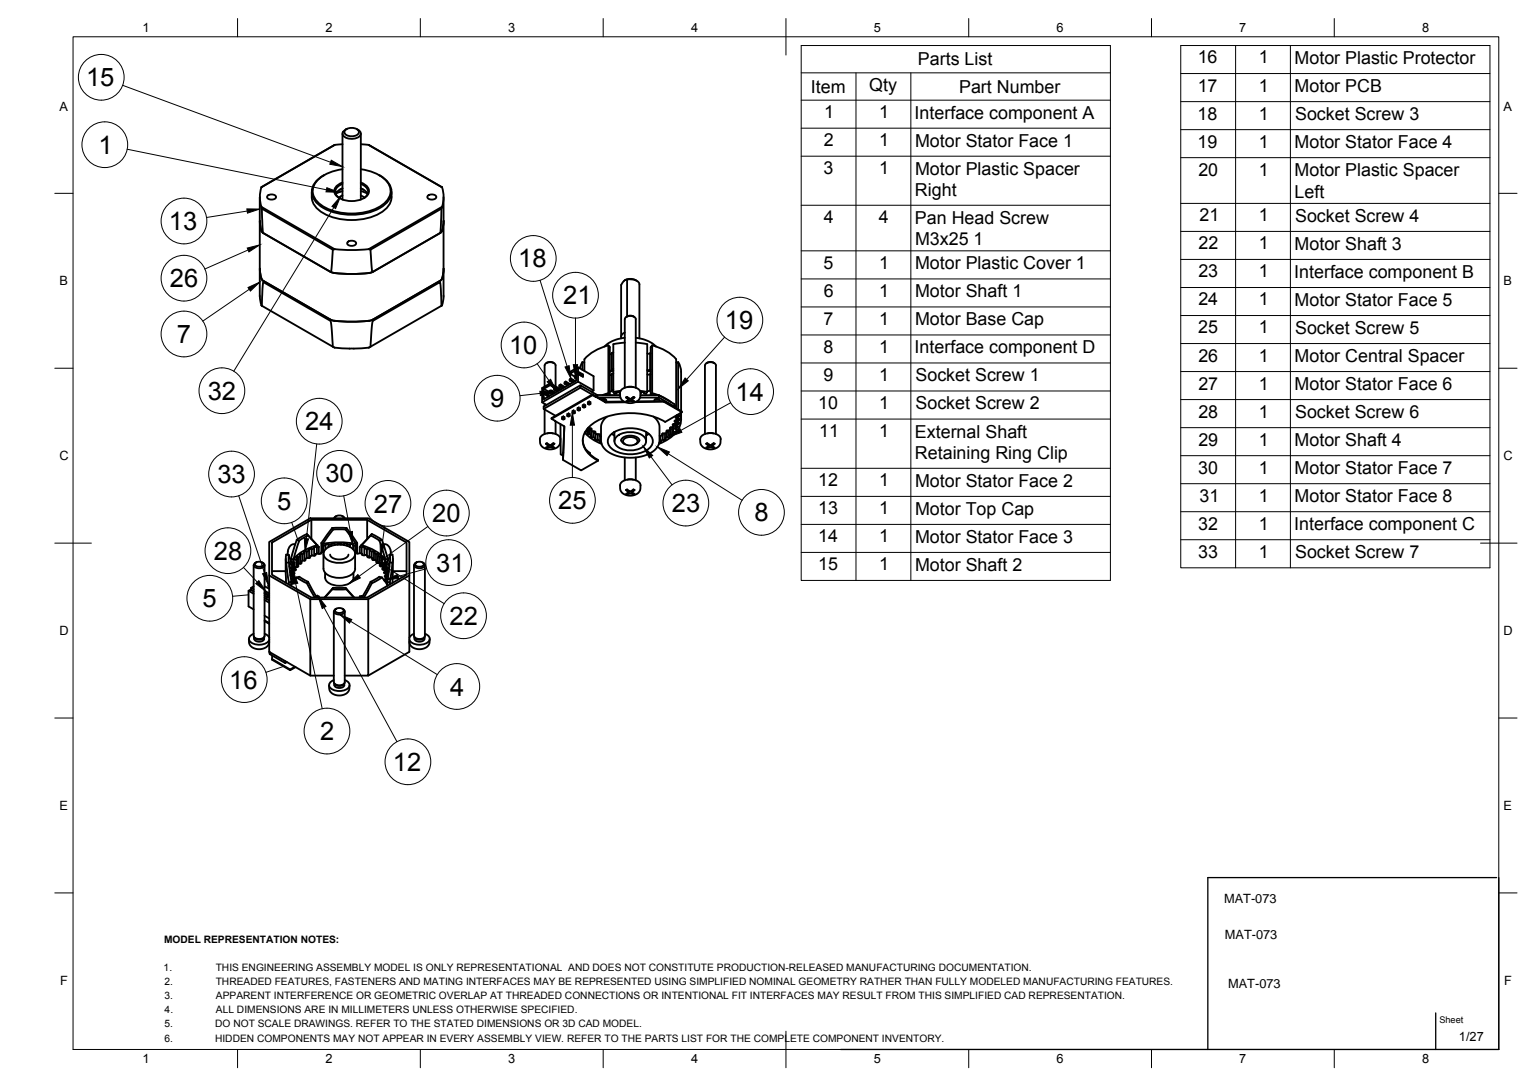
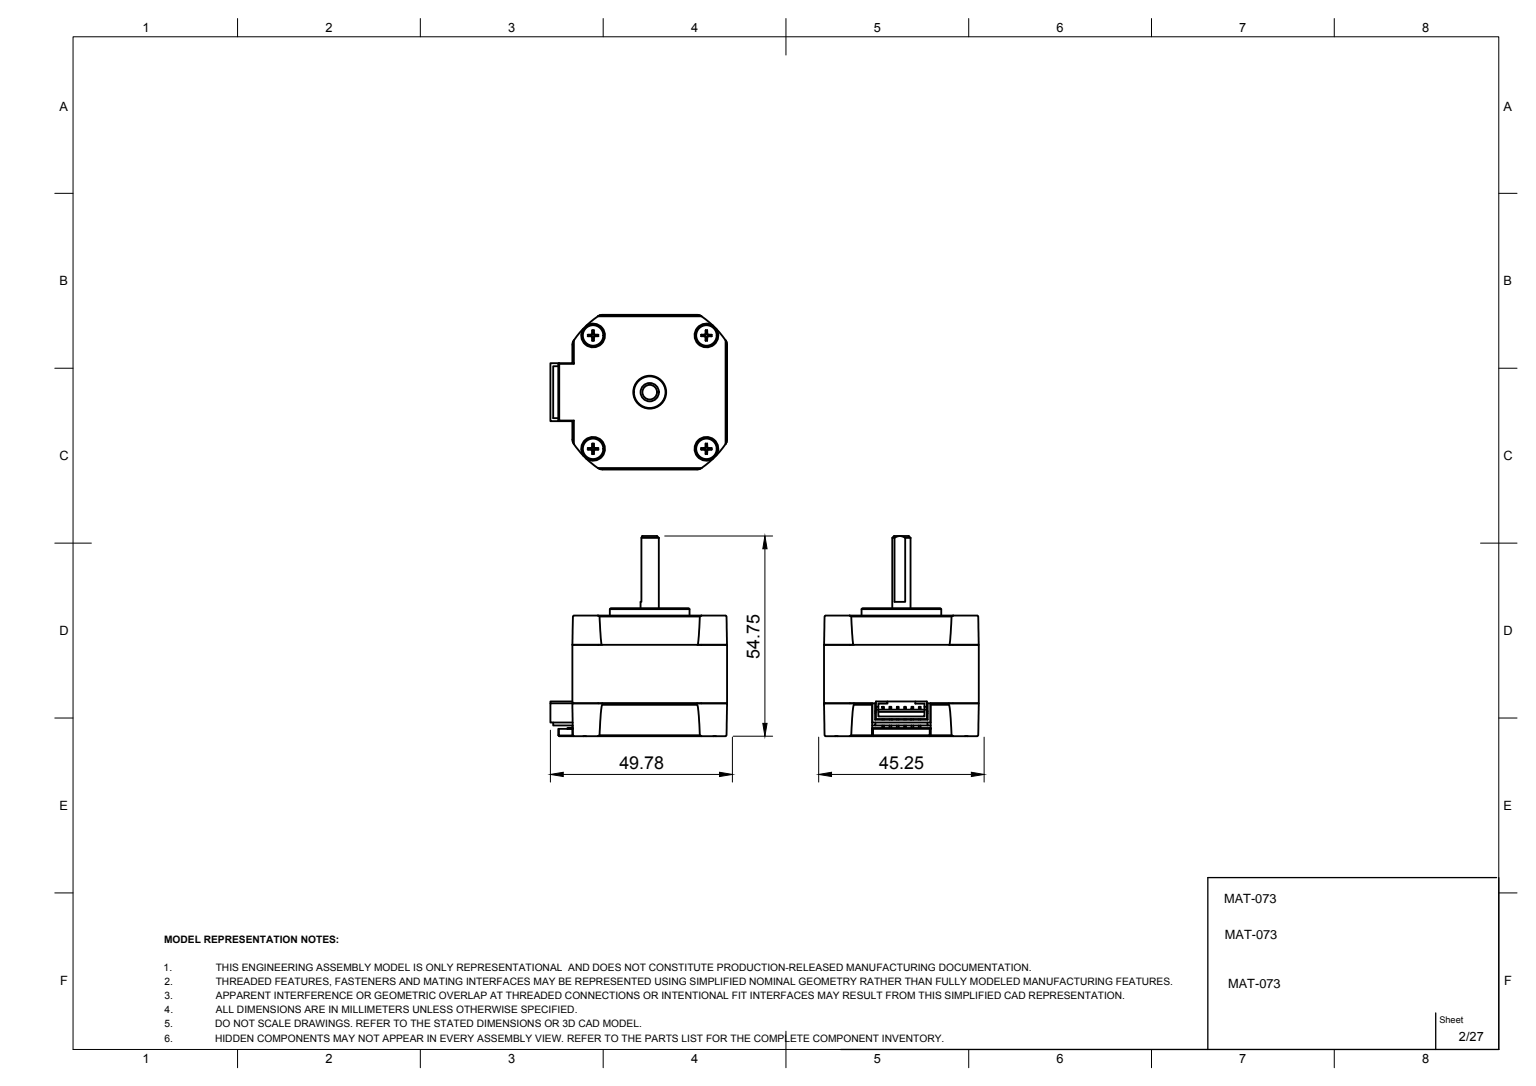
ISO-10303-21;
HEADER;
/* Generated by software containing ST-Developer
 * from STEP Tools, Inc. (www.steptools.com) 
 */

FILE_DESCRIPTION(
/* description */ ('CAx-IF Rec.Pracs.---Representation and Presentation of Product Manufa
cturing Information (PMI)---4.0---2014-10-13'),
/* implementation_level */ '2;1');

FILE_NAME(
/* name */ 'MAT-073',
/* time_stamp */ '2026-10-24T18:52:33-07:00',
/* author */ (''),
/* organization */ (''),
/* preprocessor_version */ 'ST-DEVELOPER v20.2',
/* originating_system */ 'Autodesk Translation Framework v15.17.0.0',
/* authorisation */ '');

FILE_SCHEMA (('AP242_MANAGED_MODEL_BASED_3D_ENGINEERING_MIM_LF { 1 0 10303 442 2 1 4 }'));
ENDSEC;

DATA;
#10=MECHANICAL_DESIGN_GEOMETRIC_PRESENTATION_REPRESENTATION('',(#414,#415,
#416,#417,#418,#419,#420,#421,#422,#423,#424,#425,#426,#427,#428,#429,#430,
#431,#432,#433,#434,#435,#436,#437,#438,#439,#440,#441,#442,#443,#444,#445,
#446),#34876);
#11=ITEM_DEFINED_TRANSFORMATION($,$,#19952,#22222);
#12=ITEM_DEFINED_TRANSFORMATION($,$,#19969,#22223);
#13=ITEM_DEFINED_TRANSFORMATION($,$,#20050,#22224);
#14=ITEM_DEFINED_TRANSFORMATION($,$,#22159,#22225);
#15=ITEM_DEFINED_TRANSFORMATION($,$,#20059,#22226);
#16=ITEM_DEFINED_TRANSFORMATION($,$,#20315,#22227);
#17=ITEM_DEFINED_TRANSFORMATION($,$,#20591,#22228);
#18=ITEM_DEFINED_TRANSFORMATION($,$,#20792,#22229);
#19=ITEM_DEFINED_TRANSFORMATION($,$,#20809,#22230);
#20=ITEM_DEFINED_TRANSFORMATION($,$,#20821,#22231);
#21=ITEM_DEFINED_TRANSFORMATION($,$,#20833,#22232);
#22=ITEM_DEFINED_TRANSFORMATION($,$,#20884,#22233);
#23=ITEM_DEFINED_TRANSFORMATION($,$,#20965,#22234);
#24=ITEM_DEFINED_TRANSFORMATION($,$,#21089,#22235);
#25=ITEM_DEFINED_TRANSFORMATION($,$,#21170,#22236);
#26=ITEM_DEFINED_TRANSFORMATION($,$,#21196,#22237);
#27=ITEM_DEFINED_TRANSFORMATION($,$,#21215,#22238);
#28=ITEM_DEFINED_TRANSFORMATION($,$,#21260,#22239);
#29=ITEM_DEFINED_TRANSFORMATION($,$,#21272,#22240);
#30=ITEM_DEFINED_TRANSFORMATION($,$,#21353,#22241);
#31=ITEM_DEFINED_TRANSFORMATION($,$,#21362,#22242);
#32=ITEM_DEFINED_TRANSFORMATION($,$,#21374,#22243);
#33=ITEM_DEFINED_TRANSFORMATION($,$,#21650,#22244);
#34=ITEM_DEFINED_TRANSFORMATION($,$,#21667,#22245);
#35=ITEM_DEFINED_TRANSFORMATION($,$,#21748,#22246);
#36=ITEM_DEFINED_TRANSFORMATION($,$,#21760,#22247);
#37=ITEM_DEFINED_TRANSFORMATION($,$,#21823,#22248);
#38=ITEM_DEFINED_TRANSFORMATION($,$,#21904,#22249);
#39=ITEM_DEFINED_TRANSFORMATION($,$,#21959,#22250);
#40=ITEM_DEFINED_TRANSFORMATION($,$,#21968,#22251);
#41=ITEM_DEFINED_TRANSFORMATION($,$,#22049,#22252);
#42=ITEM_DEFINED_TRANSFORMATION($,$,#22130,#22253);
#43=ITEM_DEFINED_TRANSFORMATION($,$,#22147,#22254);
#44=ITEM_DEFINED_TRANSFORMATION($,$,#22159,#22255);
#45=ITEM_DEFINED_TRANSFORMATION($,$,#22159,#22256);
#46=ITEM_DEFINED_TRANSFORMATION($,$,#22159,#22257);
#47=(
REPRESENTATION_RELATIONSHIP($,$,#34985,#34984)
REPRESENTATION_RELATIONSHIP_WITH_TRANSFORMATION(#11)
SHAPE_REPRESENTATION_RELATIONSHIP()
);
#48=(
REPRESENTATION_RELATIONSHIP($,$,#34986,#34984)
REPRESENTATION_RELATIONSHIP_WITH_TRANSFORMATION(#12)
SHAPE_REPRESENTATION_RELATIONSHIP()
);
#49=(
REPRESENTATION_RELATIONSHIP($,$,#34987,#34984)
REPRESENTATION_RELATIONSHIP_WITH_TRANSFORMATION(#13)
SHAPE_REPRESENTATION_RELATIONSHIP()
);
#50=(
REPRESENTATION_RELATIONSHIP($,$,#35017,#34984)
REPRESENTATION_RELATIONSHIP_WITH_TRANSFORMATION(#14)
SHAPE_REPRESENTATION_RELATIONSHIP()
);
#51=(
REPRESENTATION_RELATIONSHIP($,$,#34988,#34984)
REPRESENTATION_RELATIONSHIP_WITH_TRANSFORMATION(#15)
SHAPE_REPRESENTATION_RELATIONSHIP()
);
#52=(
REPRESENTATION_RELATIONSHIP($,$,#34989,#34984)
REPRESENTATION_RELATIONSHIP_WITH_TRANSFORMATION(#16)
SHAPE_REPRESENTATION_RELATIONSHIP()
);
#53=(
REPRESENTATION_RELATIONSHIP($,$,#34990,#34984)
REPRESENTATION_RELATIONSHIP_WITH_TRANSFORMATION(#17)
SHAPE_REPRESENTATION_RELATIONSHIP()
);
#54=(
REPRESENTATION_RELATIONSHIP($,$,#34991,#34984)
REPRESENTATION_RELATIONSHIP_WITH_TRANSFORMATION(#18)
SHAPE_REPRESENTATION_RELATIONSHIP()
);
#55=(
REPRESENTATION_RELATIONSHIP($,$,#34992,#34984)
REPRESENTATION_RELATIONSHIP_WITH_TRANSFORMATION(#19)
SHAPE_REPRESENTATION_RELATIONSHIP()
);
#56=(
REPRESENTATION_RELATIONSHIP($,$,#34993,#34984)
REPRESENTATION_RELATIONSHIP_WITH_TRANSFORMATION(#20)
SHAPE_REPRESENTATION_RELATIONSHIP()
);
#57=(
REPRESENTATION_RELATIONSHIP($,$,#34994,#34984)
REPRESENTATION_RELATIONSHIP_WITH_TRANSFORMATION(#21)
SHAPE_REPRESENTATION_RELATIONSHIP()
);
#58=(
REPRESENTATION_RELATIONSHIP($,$,#34995,#34984)
REPRESENTATION_RELATIONSHIP_WITH_TRANSFORMATION(#22)
SHAPE_REPRESENTATION_RELATIONSHIP()
);
#59=(
REPRESENTATION_RELATIONSHIP($,$,#34996,#34984)
REPRESENTATION_RELATIONSHIP_WITH_TRANSFORMATION(#23)
SHAPE_REPRESENTATION_RELATIONSHIP()
);
#60=(
REPRESENTATION_RELATIONSHIP($,$,#34997,#34984)
REPRESENTATION_RELATIONSHIP_WITH_TRANSFORMATION(#24)
SHAPE_REPRESENTATION_RELATIONSHIP()
);
#61=(
REPRESENTATION_RELATIONSHIP($,$,#34998,#34984)
REPRESENTATION_RELATIONSHIP_WITH_TRANSFORMATION(#25)
SHAPE_REPRESENTATION_RELATIONSHIP()
);
#62=(
REPRESENTATION_RELATIONSHIP($,$,#34999,#34984)
REPRESENTATION_RELATIONSHIP_WITH_TRANSFORMATION(#26)
SHAPE_REPRESENTATION_RELATIONSHIP()
);
#63=(
REPRESENTATION_RELATIONSHIP($,$,#35000,#34984)
REPRESENTATION_RELATIONSHIP_WITH_TRANSFORMATION(#27)
SHAPE_REPRESENTATION_RELATIONSHIP()
);
#64=(
REPRESENTATION_RELATIONSHIP($,$,#35001,#34984)
REPRESENTATION_RELATIONSHIP_WITH_TRANSFORMATION(#28)
SHAPE_REPRESENTATION_RELATIONSHIP()
);
#65=(
REPRESENTATION_RELATIONSHIP($,$,#35002,#34984)
REPRESENTATION_RELATIONSHIP_WITH_TRANSFORMATION(#29)
SHAPE_REPRESENTATION_RELATIONSHIP()
);
#66=(
REPRESENTATION_RELATIONSHIP($,$,#35003,#34984)
REPRESENTATION_RELATIONSHIP_WITH_TRANSFORMATION(#30)
SHAPE_REPRESENTATION_RELATIONSHIP()
);
#67=(
REPRESENTATION_RELATIONSHIP($,$,#35004,#34984)
REPRESENTATION_RELATIONSHIP_WITH_TRANSFORMATION(#31)
SHAPE_REPRESENTATION_RELATIONSHIP()
);
#68=(
REPRESENTATION_RELATIONSHIP($,$,#35005,#34984)
REPRESENTATION_RELATIONSHIP_WITH_TRANSFORMATION(#32)
SHAPE_REPRESENTATION_RELATIONSHIP()
);
#69=(
REPRESENTATION_RELATIONSHIP($,$,#35006,#34984)
REPRESENTATION_RELATIONSHIP_WITH_TRANSFORMATION(#33)
SHAPE_REPRESENTATION_RELATIONSHIP()
);
#70=(
REPRESENTATION_RELATIONSHIP($,$,#35007,#34984)
REPRESENTATION_RELATIONSHIP_WITH_TRANSFORMATION(#34)
SHAPE_REPRESENTATION_RELATIONSHIP()
);
#71=(
REPRESENTATION_RELATIONSHIP($,$,#35008,#34984)
REPRESENTATION_RELATIONSHIP_WITH_TRANSFORMATION(#35)
SHAPE_REPRESENTATION_RELATIONSHIP()
);
#72=(
REPRESENTATION_RELATIONSHIP($,$,#35009,#34984)
REPRESENTATION_RELATIONSHIP_WITH_TRANSFORMATION(#36)
SHAPE_REPRESENTATION_RELATIONSHIP()
);
#73=(
REPRESENTATION_RELATIONSHIP($,$,#35010,#34984)
REPRESENTATION_RELATIONSHIP_WITH_TRANSFORMATION(#37)
SHAPE_REPRESENTATION_RELATIONSHIP()
);
#74=(
REPRESENTATION_RELATIONSHIP($,$,#35011,#34984)
REPRESENTATION_RELATIONSHIP_WITH_TRANSFORMATION(#38)
SHAPE_REPRESENTATION_RELATIONSHIP()
);
#75=(
REPRESENTATION_RELATIONSHIP($,$,#35012,#34984)
REPRESENTATION_RELATIONSHIP_WITH_TRANSFORMATION(#39)
SHAPE_REPRESENTATION_RELATIONSHIP()
);
#76=(
REPRESENTATION_RELATIONSHIP($,$,#35013,#34984)
REPRESENTATION_RELATIONSHIP_WITH_TRANSFORMATION(#40)
SHAPE_REPRESENTATION_RELATIONSHIP()
);
#77=(
REPRESENTATION_RELATIONSHIP($,$,#35014,#34984)
REPRESENTATION_RELATIONSHIP_WITH_TRANSFORMATION(#41)
SHAPE_REPRESENTATION_RELATIONSHIP()
);
#78=(
REPRESENTATION_RELATIONSHIP($,$,#35015,#34984)
REPRESENTATION_RELATIONSHIP_WITH_TRANSFORMATION(#42)
SHAPE_REPRESENTATION_RELATIONSHIP()
);
#79=(
REPRESENTATION_RELATIONSHIP($,$,#35016,#34984)
REPRESENTATION_RELATIONSHIP_WITH_TRANSFORMATION(#43)
SHAPE_REPRESENTATION_RELATIONSHIP()
);
#80=(
REPRESENTATION_RELATIONSHIP($,$,#35017,#34984)
REPRESENTATION_RELATIONSHIP_WITH_TRANSFORMATION(#44)
SHAPE_REPRESENTATION_RELATIONSHIP()
);
#81=(
REPRESENTATION_RELATIONSHIP($,$,#35017,#34984)
REPRESENTATION_RELATIONSHIP_WITH_TRANSFORMATION(#45)
SHAPE_REPRESENTATION_RELATIONSHIP()
);
#82=(
REPRESENTATION_RELATIONSHIP($,$,#35017,#34984)
REPRESENTATION_RELATIONSHIP_WITH_TRANSFORMATION(#46)
SHAPE_REPRESENTATION_RELATIONSHIP()
);
#83=CONTEXT_DEPENDENT_SHAPE_REPRESENTATION(#47,#34948);
#84=CONTEXT_DEPENDENT_SHAPE_REPRESENTATION(#48,#34949);
#85=CONTEXT_DEPENDENT_SHAPE_REPRESENTATION(#49,#34950);
#86=CONTEXT_DEPENDENT_SHAPE_REPRESENTATION(#50,#34951);
#87=CONTEXT_DEPENDENT_SHAPE_REPRESENTATION(#51,#34952);
#88=CONTEXT_DEPENDENT_SHAPE_REPRESENTATION(#52,#34953);
#89=CONTEXT_DEPENDENT_SHAPE_REPRESENTATION(#53,#34954);
#90=CONTEXT_DEPENDENT_SHAPE_REPRESENTATION(#54,#34955);
#91=CONTEXT_DEPENDENT_SHAPE_REPRESENTATION(#55,#34956);
#92=CONTEXT_DEPENDENT_SHAPE_REPRESENTATION(#56,#34957);
#93=CONTEXT_DEPENDENT_SHAPE_REPRESENTATION(#57,#34958);
#94=CONTEXT_DEPENDENT_SHAPE_REPRESENTATION(#58,#34959);
#95=CONTEXT_DEPENDENT_SHAPE_REPRESENTATION(#59,#34960);
#96=CONTEXT_DEPENDENT_SHAPE_REPRESENTATION(#60,#34961);
#97=CONTEXT_DEPENDENT_SHAPE_REPRESENTATION(#61,#34962);
#98=CONTEXT_DEPENDENT_SHAPE_REPRESENTATION(#62,#34963);
#99=CONTEXT_DEPENDENT_SHAPE_REPRESENTATION(#63,#34964);
#100=CONTEXT_DEPENDENT_SHAPE_REPRESENTATION(#64,#34965);
#101=CONTEXT_DEPENDENT_SHAPE_REPRESENTATION(#65,#34966);
#102=CONTEXT_DEPENDENT_SHAPE_REPRESENTATION(#66,#34967);
#103=CONTEXT_DEPENDENT_SHAPE_REPRESENTATION(#67,#34968);
#104=CONTEXT_DEPENDENT_SHAPE_REPRESENTATION(#68,#34969);
#105=CONTEXT_DEPENDENT_SHAPE_REPRESENTATION(#69,#34970);
#106=CONTEXT_DEPENDENT_SHAPE_REPRESENTATION(#70,#34971);
#107=CONTEXT_DEPENDENT_SHAPE_REPRESENTATION(#71,#34972);
#108=CONTEXT_DEPENDENT_SHAPE_REPRESENTATION(#72,#34973);
#109=CONTEXT_DEPENDENT_SHAPE_REPRESENTATION(#73,#34974);
#110=CONTEXT_DEPENDENT_SHAPE_REPRESENTATION(#74,#34975);
#111=CONTEXT_DEPENDENT_SHAPE_REPRESENTATION(#75,#34976);
#112=CONTEXT_DEPENDENT_SHAPE_REPRESENTATION(#76,#34977);
#113=CONTEXT_DEPENDENT_SHAPE_REPRESENTATION(#77,#34978);
#114=CONTEXT_DEPENDENT_SHAPE_REPRESENTATION(#78,#34979);
#115=CONTEXT_DEPENDENT_SHAPE_REPRESENTATION(#79,#34980);
#116=CONTEXT_DEPENDENT_SHAPE_REPRESENTATION(#80,#34981);
#117=CONTEXT_DEPENDENT_SHAPE_REPRESENTATION(#81,#34982);
#118=CONTEXT_DEPENDENT_SHAPE_REPRESENTATION(#82,#34983);
#119=NEXT_ASSEMBLY_USAGE_OCCURRENCE('Interface component A:1',
'Interface component A:1','Interface component A:1',#35019,#35020,
'Interface component A:1');
#120=NEXT_ASSEMBLY_USAGE_OCCURRENCE('Motor Stator Face 1:1',
'Motor Stator Face 1:1','Motor Stator Face 1:1',#35019,#35021,
'Motor Stator Face 1:1');
#121=NEXT_ASSEMBLY_USAGE_OCCURRENCE('Motor Plastic Spacer Right:1',
'Motor Plastic Spacer Right:1','Motor Plastic Spacer Right:1',#35019,#35022,
'Motor Plastic Spacer Right:1');
#122=NEXT_ASSEMBLY_USAGE_OCCURRENCE('Pan Head Screw M3x25 1:1',
'Pan Head Screw M3x25 1:1','Pan Head Screw M3x25 1:1',#35019,#35052,
'Pan Head Screw M3x25 1:1');
#123=NEXT_ASSEMBLY_USAGE_OCCURRENCE('Motor Plastic Cover 1:1',
'Motor Plastic Cover 1:1','Motor Plastic Cover 1:1',#35019,#35023,
'Motor Plastic Cover 1:1');
#124=NEXT_ASSEMBLY_USAGE_OCCURRENCE('Motor Shaft 1:1','Motor Shaft 1:1',
'Motor Shaft 1:1',#35019,#35024,'Motor Shaft 1:1');
#125=NEXT_ASSEMBLY_USAGE_OCCURRENCE('Motor Base Cap:1',
'Motor Base Cap:1','Motor Base Cap:1',#35019,#35025,'Motor Base Cap:1');
#126=NEXT_ASSEMBLY_USAGE_OCCURRENCE('Interface component D:1',
'Interface component D:1','Interface component D:1',#35019,#35026,
'Interface component D:1');
#127=NEXT_ASSEMBLY_USAGE_OCCURRENCE('Socket Screw 1:1',
'Socket Screw 1:1','Socket Screw 1:1',#35019,#35027,'Socket Screw 1:1');
#128=NEXT_ASSEMBLY_USAGE_OCCURRENCE('Socket Screw 2:1',
'Socket Screw 2:1','Socket Screw 2:1',#35019,#35028,'Socket Screw 2:1');
#129=NEXT_ASSEMBLY_USAGE_OCCURRENCE(
'External Shaft Retaining Ring Clip:1',
'External Shaft Retaining Ring Clip:1',
'External Shaft Retaining Ring Clip:1',#35019,#35029,
'External Shaft Retaining Ring Clip:1');
#130=NEXT_ASSEMBLY_USAGE_OCCURRENCE('Motor Stator Face 2:1',
'Motor Stator Face 2:1','Motor Stator Face 2:1',#35019,#35030,
'Motor Stator Face 2:1');
#131=NEXT_ASSEMBLY_USAGE_OCCURRENCE('Motor Top Cap:1','Motor Top Cap:1',
'Motor Top Cap:1',#35019,#35031,'Motor Top Cap:1');
#132=NEXT_ASSEMBLY_USAGE_OCCURRENCE('Motor Stator Face 3:1',
'Motor Stator Face 3:1','Motor Stator Face 3:1',#35019,#35032,
'Motor Stator Face 3:1');
#133=NEXT_ASSEMBLY_USAGE_OCCURRENCE('Motor Shaft 2:1','Motor Shaft 2:1',
'Motor Shaft 2:1',#35019,#35033,'Motor Shaft 2:1');
#134=NEXT_ASSEMBLY_USAGE_OCCURRENCE('Motor Plastic Protector:1',
'Motor Plastic Protector:1','Motor Plastic Protector:1',#35019,#35034,
'Motor Plastic Protector:1');
#135=NEXT_ASSEMBLY_USAGE_OCCURRENCE('Motor PCB:1','Motor PCB:1',
'Motor PCB:1',#35019,#35035,'Motor PCB:1');
#136=NEXT_ASSEMBLY_USAGE_OCCURRENCE('Socket Screw 3:1',
'Socket Screw 3:1','Socket Screw 3:1',#35019,#35036,'Socket Screw 3:1');
#137=NEXT_ASSEMBLY_USAGE_OCCURRENCE('Motor Stator Face 4:1',
'Motor Stator Face 4:1','Motor Stator Face 4:1',#35019,#35037,
'Motor Stator Face 4:1');
#138=NEXT_ASSEMBLY_USAGE_OCCURRENCE('Motor Plastic Spacer Left:1',
'Motor Plastic Spacer Left:1','Motor Plastic Spacer Left:1',#35019,#35038,
'Motor Plastic Spacer Left:1');
#139=NEXT_ASSEMBLY_USAGE_OCCURRENCE('Socket Screw 4:1',
'Socket Screw 4:1','Socket Screw 4:1',#35019,#35039,'Socket Screw 4:1');
#140=NEXT_ASSEMBLY_USAGE_OCCURRENCE('Motor Shaft 3:1','Motor Shaft 3:1',
'Motor Shaft 3:1',#35019,#35040,'Motor Shaft 3:1');
#141=NEXT_ASSEMBLY_USAGE_OCCURRENCE('Interface component B:1',
'Interface component B:1','Interface component B:1',#35019,#35041,
'Interface component B:1');
#142=NEXT_ASSEMBLY_USAGE_OCCURRENCE('Motor Stator Face 5:1',
'Motor Stator Face 5:1','Motor Stator Face 5:1',#35019,#35042,
'Motor Stator Face 5:1');
#143=NEXT_ASSEMBLY_USAGE_OCCURRENCE('Socket Screw 5:1',
'Socket Screw 5:1','Socket Screw 5:1',#35019,#35043,'Socket Screw 5:1');
#144=NEXT_ASSEMBLY_USAGE_OCCURRENCE('Motor Central Spacer:1',
'Motor Central Spacer:1','Motor Central Spacer:1',#35019,#35044,
'Motor Central Spacer:1');
#145=NEXT_ASSEMBLY_USAGE_OCCURRENCE('Motor Stator Face 6:1',
'Motor Stator Face 6:1','Motor Stator Face 6:1',#35019,#35045,
'Motor Stator Face 6:1');
#146=NEXT_ASSEMBLY_USAGE_OCCURRENCE('Socket Screw 6:1',
'Socket Screw 6:1','Socket Screw 6:1',#35019,#35046,'Socket Screw 6:1');
#147=NEXT_ASSEMBLY_USAGE_OCCURRENCE('Motor Shaft 4:1','Motor Shaft 4:1',
'Motor Shaft 4:1',#35019,#35047,'Motor Shaft 4:1');
#148=NEXT_ASSEMBLY_USAGE_OCCURRENCE('Motor Stator Face 7:1',
'Motor Stator Face 7:1','Motor Stator Face 7:1',#35019,#35048,
'Motor Stator Face 7:1');
#149=NEXT_ASSEMBLY_USAGE_OCCURRENCE('Motor Stator Face 8:1',
'Motor Stator Face 8:1','Motor Stator Face 8:1',#35019,#35049,
'Motor Stator Face 8:1');
#150=NEXT_ASSEMBLY_USAGE_OCCURRENCE('Interface component C:1',
'Interface component C:1','Interface component C:1',#35019,#35050,
'Interface component C:1');
#151=NEXT_ASSEMBLY_USAGE_OCCURRENCE('Socket Screw 7:1',
'Socket Screw 7:1','Socket Screw 7:1',#35019,#35051,'Socket Screw 7:1');
#152=NEXT_ASSEMBLY_USAGE_OCCURRENCE('Pan Head Screw M3x25 1:2',
'Pan Head Screw M3x25 1:2','Pan Head Screw M3x25 1:2',#35019,#35052,
'Pan Head Screw M3x25 1:2');
#153=NEXT_ASSEMBLY_USAGE_OCCURRENCE('Pan Head Screw M3x25 1:3',
'Pan Head Screw M3x25 1:3','Pan Head Screw M3x25 1:3',#35019,#35052,
'Pan Head Screw M3x25 1:3');
#154=NEXT_ASSEMBLY_USAGE_OCCURRENCE('Pan Head Screw M3x25 1:4',
'Pan Head Screw M3x25 1:4','Pan Head Screw M3x25 1:4',#35019,#35052,
'Pan Head Screw M3x25 1:4');
#155=SPHERICAL_SURFACE('',#22193,0.005);
#156=(
BOUNDED_CURVE()
B_SPLINE_CURVE(2,(#31813,#31814,#31815),.UNSPECIFIED.,.F.,.F.)
B_SPLINE_CURVE_WITH_KNOTS((3,3),(0.,0.159611859165466),.UNSPECIFIED.)
CURVE()
GEOMETRIC_REPRESENTATION_ITEM()
RATIONAL_B_SPLINE_CURVE((1.,1.06066017177976,1.))
REPRESENTATION_ITEM('')
);
#157=(
BOUNDED_CURVE()
B_SPLINE_CURVE(2,(#31820,#31821,#31822),.UNSPECIFIED.,.F.,.F.)
B_SPLINE_CURVE_WITH_KNOTS((3,3),(0.159611859165466,0.319223718330933),
 .UNSPECIFIED.)
CURVE()
GEOMETRIC_REPRESENTATION_ITEM()
RATIONAL_B_SPLINE_CURVE((1.,1.06066017177976,1.))
REPRESENTATION_ITEM('')
);
#158=(
BOUNDED_CURVE()
B_SPLINE_CURVE(2,(#34461,#34462,#34463),.UNSPECIFIED.,.F.,.F.)
B_SPLINE_CURVE_WITH_KNOTS((3,3),(0.0607926731753692,0.157120419745457),
 .UNSPECIFIED.)
CURVE()
GEOMETRIC_REPRESENTATION_ITEM()
RATIONAL_B_SPLINE_CURVE((1.16988778338128,1.27990737092129,1.3120427295614))
REPRESENTATION_ITEM('')
);
#159=(
BOUNDED_CURVE()
B_SPLINE_CURVE(2,(#34466,#34467,#34468),.UNSPECIFIED.,.F.,.F.)
B_SPLINE_CURVE_WITH_KNOTS((3,3),(0.236610881719778,0.332938628428626),
 .UNSPECIFIED.)
CURVE()
GEOMETRIC_REPRESENTATION_ITEM()
RATIONAL_B_SPLINE_CURVE((1.3120427260588,1.27990736807416,1.16988778190421))
REPRESENTATION_ITEM('')
);
#160=(
BOUNDED_CURVE()
B_SPLINE_CURVE(2,(#34498,#34499,#34500),.UNSPECIFIED.,.F.,.F.)
B_SPLINE_CURVE_WITH_KNOTS((3,3),(0.060792673372948,0.15712042005291),
 .UNSPECIFIED.)
CURVE()
GEOMETRIC_REPRESENTATION_ITEM()
RATIONAL_B_SPLINE_CURVE((1.16988778221416,1.2799073686718,1.31204272679384))
REPRESENTATION_ITEM('')
);
#161=(
BOUNDED_CURVE()
B_SPLINE_CURVE(2,(#34503,#34504,#34505),.UNSPECIFIED.,.F.,.F.)
B_SPLINE_CURVE_WITH_KNOTS((3,3),(0.236610881752925,0.332938628449716),
 .UNSPECIFIED.)
CURVE()
GEOMETRIC_REPRESENTATION_ITEM()
RATIONAL_B_SPLINE_CURVE((1.3120427263507,1.27990736831095,1.16988778202699))
REPRESENTATION_ITEM('')
);
#162=(
BOUNDED_CURVE()
B_SPLINE_CURVE(2,(#34535,#34536,#34537),.UNSPECIFIED.,.F.,.F.)
B_SPLINE_CURVE_WITH_KNOTS((3,3),(0.0607926734092304,0.157120420109433),
 .UNSPECIFIED.)
CURVE()
GEOMETRIC_REPRESENTATION_ITEM()
RATIONAL_B_SPLINE_CURVE((1.1698877820014,1.27990736826137,1.31204272628854))
REPRESENTATION_ITEM('')
);
#163=(
BOUNDED_CURVE()
B_SPLINE_CURVE(2,(#34542,#34543,#34544),.UNSPECIFIED.,.F.,.F.)
B_SPLINE_CURVE_WITH_KNOTS((3,3),(0.23661088156082,0.33293862832676),
 .UNSPECIFIED.)
CURVE()
GEOMETRIC_REPRESENTATION_ITEM()
RATIONAL_B_SPLINE_CURVE((1.31204272463436,1.27990736691681,1.16988778130364))
REPRESENTATION_ITEM('')
);
#164=(
BOUNDED_CURVE()
B_SPLINE_CURVE(2,(#34574,#34575,#34576),.UNSPECIFIED.,.F.,.F.)
B_SPLINE_CURVE_WITH_KNOTS((3,3),(0.0607926733478611,0.157120420013774),
 .UNSPECIFIED.)
CURVE()
GEOMETRIC_REPRESENTATION_ITEM()
RATIONAL_B_SPLINE_CURVE((1.16988778236303,1.27990736895843,1.31204272714642))
REPRESENTATION_ITEM('')
);
#165=(
BOUNDED_CURVE()
B_SPLINE_CURVE(2,(#34579,#34580,#34581),.UNSPECIFIED.,.F.,.F.)
B_SPLINE_CURVE_WITH_KNOTS((3,3),(0.236610882341047,0.332938628827773),
 .UNSPECIFIED.)
CURVE()
GEOMETRIC_REPRESENTATION_ITEM()
RATIONAL_B_SPLINE_CURVE((1.3120427316459,1.27990737261498,1.16988778425995))
REPRESENTATION_ITEM('')
);
#166=(
BOUNDED_CURVE()
B_SPLINE_CURVE(2,(#34671,#34672,#34673),.UNSPECIFIED.,.F.,.F.)
B_SPLINE_CURVE_WITH_KNOTS((3,3),(0.167664209749899,0.177304440757115),
 .UNSPECIFIED.)
CURVE()
GEOMETRIC_REPRESENTATION_ITEM()
RATIONAL_B_SPLINE_CURVE((1.60521077046129,1.32000436275842,1.))
REPRESENTATION_ITEM('')
);
#167=(
BOUNDED_CURVE()
B_SPLINE_CURVE(2,(#34677,#34678,#34679),.UNSPECIFIED.,.F.,.F.)
B_SPLINE_CURVE_WITH_KNOTS((3,3),(0.,0.0096402310072164),.UNSPECIFIED.)
CURVE()
GEOMETRIC_REPRESENTATION_ITEM()
RATIONAL_B_SPLINE_CURVE((1.,1.32000436275842,1.60521077046128))
REPRESENTATION_ITEM('')
);
#168=(
BOUNDED_CURVE()
B_SPLINE_CURVE(2,(#34699,#34700,#34701),.UNSPECIFIED.,.F.,.F.)
B_SPLINE_CURVE_WITH_KNOTS((3,3),(0.167664209749899,0.177304440757115),
 .UNSPECIFIED.)
CURVE()
GEOMETRIC_REPRESENTATION_ITEM()
RATIONAL_B_SPLINE_CURVE((1.60521077046129,1.32000436275842,1.))
REPRESENTATION_ITEM('')
);
#169=(
BOUNDED_CURVE()
B_SPLINE_CURVE(2,(#34704,#34705,#34706),.UNSPECIFIED.,.F.,.F.)
B_SPLINE_CURVE_WITH_KNOTS((3,3),(0.167664209749899,0.177304440757115),
 .UNSPECIFIED.)
CURVE()
GEOMETRIC_REPRESENTATION_ITEM()
RATIONAL_B_SPLINE_CURVE((1.60521077046128,1.32000436275842,1.))
REPRESENTATION_ITEM('')
);
#170=(
BOUNDED_CURVE()
B_SPLINE_CURVE(2,(#34708,#34709,#34710),.UNSPECIFIED.,.F.,.F.)
B_SPLINE_CURVE_WITH_KNOTS((3,3),(0.,0.00964023100721641),.UNSPECIFIED.)
CURVE()
GEOMETRIC_REPRESENTATION_ITEM()
RATIONAL_B_SPLINE_CURVE((1.,1.32000436275842,1.60521077046128))
REPRESENTATION_ITEM('')
);
#171=(
BOUNDED_CURVE()
B_SPLINE_CURVE(2,(#34713,#34714,#34715),.UNSPECIFIED.,.F.,.F.)
B_SPLINE_CURVE_WITH_KNOTS((3,3),(0.167664209749899,0.177304440757115),
 .UNSPECIFIED.)
CURVE()
GEOMETRIC_REPRESENTATION_ITEM()
RATIONAL_B_SPLINE_CURVE((1.60521077046128,1.32000436275842,1.))
REPRESENTATION_ITEM('')
);
#172=(
BOUNDED_CURVE()
B_SPLINE_CURVE(2,(#34720,#34721,#34722),.UNSPECIFIED.,.F.,.F.)
B_SPLINE_CURVE_WITH_KNOTS((3,3),(0.,0.00964023100721641),.UNSPECIFIED.)
CURVE()
GEOMETRIC_REPRESENTATION_ITEM()
RATIONAL_B_SPLINE_CURVE((1.,1.32000436275842,1.60521077046128))
REPRESENTATION_ITEM('')
);
#173=(
BOUNDED_CURVE()
B_SPLINE_CURVE(2,(#34756,#34757,#34758),.UNSPECIFIED.,.F.,.F.)
B_SPLINE_CURVE_WITH_KNOTS((3,3),(0.,0.0096402310072164),.UNSPECIFIED.)
CURVE()
GEOMETRIC_REPRESENTATION_ITEM()
RATIONAL_B_SPLINE_CURVE((1.,1.32000436275842,1.60521077046128))
REPRESENTATION_ITEM('')
);
#174=CONICAL_SURFACE('',#20658,0.003125,0.785398163397447);
#175=CONICAL_SURFACE('',#20665,0.003125,0.785398163397447);
#176=CONICAL_SURFACE('',#20672,0.003125,0.785398163397447);
#177=CONICAL_SURFACE('',#20689,0.003125,0.785398163397447);
#178=CONICAL_SURFACE('',#20758,0.012875,0.785398163397446);
#179=CONICAL_SURFACE('',#20765,0.008125,0.244978663126864);
#180=CONICAL_SURFACE('',#21050,0.010775,0.785398163397447);
#181=CONICAL_SURFACE('',#21057,0.004625,0.785398163397445);
#182=CONICAL_SURFACE('',#21062,0.004625,0.785398163397443);
#183=CONICAL_SURFACE('',#21066,0.012875,0.785398163397446);
#184=CONICAL_SURFACE('',#21072,0.008125,0.244978663126864);
#185=CONICAL_SURFACE('',#21171,0.00225,0.78539816339745);
#186=CONICAL_SURFACE('',#21175,0.00225,0.78539816339745);
#187=CONICAL_SURFACE('',#21192,0.00225,0.78539816339745);
#188=CONICAL_SURFACE('',#22160,0.0013466375,0.785235177497158);
#189=CONICAL_SURFACE('',#22170,0.00111007998137123,0.462512251778497);
#190=CONICAL_SURFACE('',#22175,0.00111007998137123,0.462512251778497);
#191=CONICAL_SURFACE('',#22180,0.00111007998137123,0.462512251778497);
#192=CONICAL_SURFACE('',#22186,0.00111007998137123,0.462512251778497);
#193=CONICAL_SURFACE('',#22202,0.00277242641351798,0.0349065850398864);
#194=CONICAL_SURFACE('',#22204,0.000209529102193857,0.0872664625997164);
#195=CONICAL_SURFACE('',#22207,0.000209529102193857,0.0872664625997164);
#196=CONICAL_SURFACE('',#22213,0.000209529102193857,0.0872664625997164);
#197=CONICAL_SURFACE('',#22214,0.000209529102193857,0.0872664625997164);
#198=CONICAL_SURFACE('',#22216,0.000409956151237738,1.08210413623649);
#199=CONICAL_SURFACE('',#22221,0.0014323425,0.415478851838033);
#200=B_SPLINE_CURVE_WITH_KNOTS('',3,(#28743,#28744,#28745,#28746,#28747,
#28748,#28749,#28750,#28751,#28752,#28753,#28754,#28755,#28756,#28757,#28758,
#28759,#28760),.UNSPECIFIED.,.F.,.F.,(4,2,2,2,2,2,2,2,4),(-0.452364390465681,
-0.395818735844292,-0.339273081222902,-0.282727638227872,-0.226182195232841,
-0.16963675223781,-0.113091309242778,-0.0565456546213892,0.),
 .UNSPECIFIED.);
#201=B_SPLINE_CURVE_WITH_KNOTS('',3,(#28763,#28764,#28765,#28766,#28767,
#28768,#28769,#28770,#28771,#28772,#28773,#28774,#28775,#28776,#28777,#28778,
#28779,#28780),.UNSPECIFIED.,.F.,.F.,(4,2,2,2,2,2,2,2,4),(-0.904728780931361,
-0.848183126309972,-0.791637471688583,-0.735092028693552,-0.678546585698521,
-0.62200114270349,-0.565455699708459,-0.50891004508707,-0.452364390465681),
 .UNSPECIFIED.);
#202=B_SPLINE_CURVE_WITH_KNOTS('',3,(#28851,#28852,#28853,#28854,#28855,
#28856,#28857,#28858,#28859,#28860,#28861,#28862,#28863,#28864,#28865,#28866,
#28867,#28868),.UNSPECIFIED.,.F.,.F.,(4,2,2,2,2,2,2,2,4),(-0.452364390465681,
-0.395818735844292,-0.339273081222903,-0.282727638227872,-0.22618219523284,
-0.169636752237809,-0.113091309242778,-0.0565456546213892,0.),
 .UNSPECIFIED.);
#203=B_SPLINE_CURVE_WITH_KNOTS('',3,(#28871,#28872,#28873,#28874,#28875,
#28876,#28877,#28878,#28879,#28880,#28881,#28882,#28883,#28884,#28885,#28886,
#28887,#28888),.UNSPECIFIED.,.F.,.F.,(4,2,2,2,2,2,2,2,4),(-0.904728780931361,
-0.848183126309972,-0.791637471688583,-0.735092028693552,-0.678546585698521,
-0.622001142703489,-0.565455699708458,-0.508910045087069,-0.45236439046568),
 .UNSPECIFIED.);
#204=B_SPLINE_CURVE_WITH_KNOTS('',3,(#28959,#28960,#28961,#28962,#28963,
#28964,#28965,#28966,#28967,#28968,#28969,#28970,#28971,#28972,#28973,#28974,
#28975,#28976),.UNSPECIFIED.,.F.,.F.,(4,2,2,2,2,2,2,2,4),(-0.452364390465681,
-0.395818735844292,-0.339273081222902,-0.282727638227871,-0.22618219523284,
-0.169636752237809,-0.113091309242778,-0.0565456546213892,0.),
 .UNSPECIFIED.);
#205=B_SPLINE_CURVE_WITH_KNOTS('',3,(#28979,#28980,#28981,#28982,#28983,
#28984,#28985,#28986,#28987,#28988,#28989,#28990,#28991,#28992,#28993,#28994,
#28995,#28996),.UNSPECIFIED.,.F.,.F.,(4,2,2,2,2,2,2,2,4),(-0.904728780931362,
-0.848183126309972,-0.791637471688583,-0.735092028693552,-0.678546585698521,
-0.62200114270349,-0.565455699708459,-0.50891004508707,-0.452364390465681),
 .UNSPECIFIED.);
#206=B_SPLINE_CURVE_WITH_KNOTS('',3,(#29067,#29068,#29069,#29070,#29071,
#29072,#29073,#29074,#29075,#29076,#29077,#29078,#29079,#29080,#29081,#29082,
#29083,#29084),.UNSPECIFIED.,.F.,.F.,(4,2,2,2,2,2,2,2,4),(-0.452364390465681,
-0.395818735844292,-0.339273081222903,-0.282727638227872,-0.226182195232841,
-0.169636752237809,-0.113091309242778,-0.0565456546213892,0.),
 .UNSPECIFIED.);
#207=B_SPLINE_CURVE_WITH_KNOTS('',3,(#29087,#29088,#29089,#29090,#29091,
#29092,#29093,#29094,#29095,#29096,#29097,#29098,#29099,#29100,#29101,#29102,
#29103,#29104),.UNSPECIFIED.,.F.,.F.,(4,2,2,2,2,2,2,2,4),(-0.904728780931362,
-0.848183126309973,-0.791637471688583,-0.735092028693552,-0.678546585698521,
-0.62200114270349,-0.565455699708459,-0.50891004508707,-0.452364390465681),
 .UNSPECIFIED.);
#208=B_SPLINE_CURVE_WITH_KNOTS('',3,(#29175,#29176,#29177,#29178,#29179,
#29180,#29181,#29182,#29183,#29184,#29185,#29186,#29187,#29188,#29189,#29190,
#29191,#29192),.UNSPECIFIED.,.F.,.F.,(4,2,2,2,2,2,2,2,4),(-0.452364390465681,
-0.395818735844292,-0.339273081222903,-0.282727638227872,-0.226182195232841,
-0.169636752237809,-0.113091309242778,-0.0565456546213892,0.),
 .UNSPECIFIED.);
#209=B_SPLINE_CURVE_WITH_KNOTS('',3,(#29195,#29196,#29197,#29198,#29199,
#29200,#29201,#29202,#29203,#29204,#29205,#29206,#29207,#29208,#29209,#29210,
#29211,#29212),.UNSPECIFIED.,.F.,.F.,(4,2,2,2,2,2,2,2,4),(-0.904728780931362,
-0.848183126309973,-0.791637471688584,-0.735092028693553,-0.678546585698522,
-0.62200114270349,-0.565455699708459,-0.50891004508707,-0.452364390465681),
 .UNSPECIFIED.);
#210=B_SPLINE_CURVE_WITH_KNOTS('',3,(#29283,#29284,#29285,#29286,#29287,
#29288,#29289,#29290,#29291,#29292,#29293,#29294,#29295,#29296,#29297,#29298,
#29299,#29300),.UNSPECIFIED.,.F.,.F.,(4,2,2,2,2,2,2,2,4),(-0.452364390465681,
-0.395818735844292,-0.339273081222903,-0.282727638227872,-0.22618219523284,
-0.169636752237809,-0.113091309242778,-0.0565456546213891,0.),
 .UNSPECIFIED.);
#211=B_SPLINE_CURVE_WITH_KNOTS('',3,(#29303,#29304,#29305,#29306,#29307,
#29308,#29309,#29310,#29311,#29312,#29313,#29314,#29315,#29316,#29317,#29318,
#29319,#29320),.UNSPECIFIED.,.F.,.F.,(4,2,2,2,2,2,2,2,4),(-0.904728780931362,
-0.848183126309973,-0.791637471688583,-0.735092028693552,-0.678546585698521,
-0.62200114270349,-0.565455699708459,-0.50891004508707,-0.452364390465681),
 .UNSPECIFIED.);
#212=B_SPLINE_CURVE_WITH_KNOTS('',3,(#29391,#29392,#29393,#29394,#29395,
#29396,#29397,#29398,#29399,#29400,#29401,#29402,#29403,#29404,#29405,#29406,
#29407,#29408),.UNSPECIFIED.,.F.,.F.,(4,2,2,2,2,2,2,2,4),(-0.452364390465681,
-0.395818735844292,-0.339273081222902,-0.282727638227872,-0.226182195232841,
-0.169636752237809,-0.113091309242778,-0.0565456546213892,0.),
 .UNSPECIFIED.);
#213=B_SPLINE_CURVE_WITH_KNOTS('',3,(#29411,#29412,#29413,#29414,#29415,
#29416,#29417,#29418,#29419,#29420,#29421,#29422,#29423,#29424,#29425,#29426,
#29427,#29428),.UNSPECIFIED.,.F.,.F.,(4,2,2,2,2,2,2,2,4),(-0.904728780931362,
-0.848183126309973,-0.791637471688583,-0.735092028693552,-0.678546585698521,
-0.62200114270349,-0.565455699708459,-0.50891004508707,-0.452364390465681),
 .UNSPECIFIED.);
#214=B_SPLINE_CURVE_WITH_KNOTS('',3,(#29499,#29500,#29501,#29502,#29503,
#29504,#29505,#29506,#29507,#29508,#29509,#29510,#29511,#29512,#29513,#29514,
#29515,#29516),.UNSPECIFIED.,.F.,.F.,(4,2,2,2,2,2,2,2,4),(-0.452364390465681,
-0.395818735844292,-0.339273081222903,-0.282727638227872,-0.226182195232841,
-0.169636752237809,-0.113091309242778,-0.0565456546213892,0.),
 .UNSPECIFIED.);
#215=B_SPLINE_CURVE_WITH_KNOTS('',3,(#29519,#29520,#29521,#29522,#29523,
#29524,#29525,#29526,#29527,#29528,#29529,#29530,#29531,#29532,#29533,#29534,
#29535,#29536),.UNSPECIFIED.,.F.,.F.,(4,2,2,2,2,2,2,2,4),(-0.904728780931362,
-0.848183126309973,-0.791637471688583,-0.735092028693552,-0.678546585698521,
-0.62200114270349,-0.565455699708459,-0.50891004508707,-0.452364390465681),
 .UNSPECIFIED.);
#216=B_SPLINE_CURVE_WITH_KNOTS('',3,(#30332,#30333,#30334,#30335,#30336,
#30337),.UNSPECIFIED.,.F.,.F.,(4,2,4),(1.58777834959488,1.67090244580867,
1.70100758687363),.UNSPECIFIED.);
#217=B_SPLINE_CURVE_WITH_KNOTS('',3,(#30373,#30374,#30375,#30376,#30377,
#30378),.UNSPECIFIED.,.F.,.F.,(4,2,4),(1.58777834958732,1.67090244580931,
1.70100758688213),.UNSPECIFIED.);
#218=B_SPLINE_CURVE_WITH_KNOTS('',3,(#30414,#30415,#30416,#30417,#30418,
#30419),.UNSPECIFIED.,.F.,.F.,(4,2,4),(1.58777834957897,1.67090244581023,
1.70100758689154),.UNSPECIFIED.);
#219=B_SPLINE_CURVE_WITH_KNOTS('',3,(#30471,#30472,#30473,#30474,#30475,
#30476),.UNSPECIFIED.,.F.,.F.,(4,2,4),(1.58777834959617,1.67090244580851,
1.70100758687202),.UNSPECIFIED.);
#220=B_SPLINE_CURVE_WITH_KNOTS('',3,(#34435,#34436,#34437,#34438,#34439,
#34440,#34441,#34442,#34443,#34444),.UNSPECIFIED.,.F.,.F.,(4,2,2,2,4),(0.0294844094794275,
0.0320672178808003,0.0352683618118342,0.0385150894591433,0.0409598490463399),
 .UNSPECIFIED.);
#221=B_SPLINE_CURVE_WITH_KNOTS('',3,(#34448,#34449,#34450,#34451,#34452,
#34453,#34454,#34455,#34456,#34457),.UNSPECIFIED.,.F.,.F.,(4,2,2,2,4),(0.0104731770181891,
0.0129179366053853,0.0161646642526944,0.0193658081837281,0.0219486165852225),
 .UNSPECIFIED.);
#222=B_SPLINE_CURVE_WITH_KNOTS('',3,(#34472,#34473,#34474,#34475,#34476,
#34477,#34478,#34479,#34480,#34481),.UNSPECIFIED.,.F.,.F.,(4,2,2,2,4),(0.0294844112755818,
0.0320672196769547,0.0352683636079885,0.0385150912552978,0.0409598508424944),
 .UNSPECIFIED.);
#223=B_SPLINE_CURVE_WITH_KNOTS('',3,(#34485,#34486,#34487,#34488,#34489,
#34490,#34491,#34492,#34493,#34494),.UNSPECIFIED.,.F.,.F.,(4,2,2,2,4),(0.0104731770181892,
0.0129179366053856,0.0161646642526945,0.0193658081837283,0.0219486165852223),
 .UNSPECIFIED.);
#224=B_SPLINE_CURVE_WITH_KNOTS('',3,(#34509,#34510,#34511,#34512,#34513,
#34514,#34515,#34516,#34517,#34518),.UNSPECIFIED.,.F.,.F.,(4,2,2,2,4),(0.0294844112754596,
0.0320672196769543,0.0352683636079882,0.0385150912552974,0.040959850842494),
 .UNSPECIFIED.);
#225=B_SPLINE_CURVE_WITH_KNOTS('',3,(#34522,#34523,#34524,#34525,#34526,
#34527,#34528,#34529,#34530,#34531),.UNSPECIFIED.,.F.,.F.,(4,2,2,2,4),(0.0104731770181891,
0.0129179366053853,0.0161646642526943,0.0193658081837282,0.0219486165851014),
 .UNSPECIFIED.);
#226=B_SPLINE_CURVE_WITH_KNOTS('',3,(#34548,#34549,#34550,#34551,#34552,
#34553,#34554,#34555,#34556,#34557),.UNSPECIFIED.,.F.,.F.,(4,2,2,2,4),(0.029484409479306,
0.0320672178808001,0.0352683618118339,0.038515089459143,0.0409598490463398),
 .UNSPECIFIED.);
#227=B_SPLINE_CURVE_WITH_KNOTS('',3,(#34561,#34562,#34563,#34564,#34565,
#34566,#34567,#34568,#34569,#34570),.UNSPECIFIED.,.F.,.F.,(4,2,2,2,4),(0.0104731770181892,
0.0129179366053856,0.0161646642526945,0.0193658081837283,0.0219486165851011),
 .UNSPECIFIED.);
#228=B_SPLINE_CURVE_WITH_KNOTS('',3,(#34594,#34595,#34596,#34597,#34598,
#34599,#34600,#34601,#34602,#34603),.UNSPECIFIED.,.F.,.F.,(4,2,2,2,4),(0.0992219002317977,
0.105487377923686,0.113471050376119,0.121445475099517,0.129419899822916),
 .UNSPECIFIED.);
#229=B_SPLINE_CURVE_WITH_KNOTS('',3,(#34608,#34609,#34610,#34611,#34612,
#34613,#34614,#34615,#34616,#34617),.UNSPECIFIED.,.F.,.F.,(4,2,2,2,4),(0.0992219004931051,
0.105487378184993,0.113471050637426,0.121445475360824,0.129419900084223),
 .UNSPECIFIED.);
#230=B_SPLINE_CURVE_WITH_KNOTS('',3,(#34622,#34623,#34624,#34625,#34626,
#34627,#34628,#34629,#34630,#34631),.UNSPECIFIED.,.F.,.F.,(4,2,2,2,4),(0.099221900231798,
0.105487377923686,0.113471050376119,0.121445475099517,0.129419899822916),
 .UNSPECIFIED.);
#231=B_SPLINE_CURVE_WITH_KNOTS('',3,(#34636,#34637,#34638,#34639,#34640,
#34641,#34642,#34643,#34644,#34645),.UNSPECIFIED.,.F.,.F.,(4,2,2,2,4),(0.0992219004931048,
0.105487378184993,0.113471050637426,0.121445475360825,0.129419900084223),
 .UNSPECIFIED.);
#232=B_SPLINE_CURVE_WITH_KNOTS('',3,(#34655,#34656,#34657,#34658,#34659,
#34660,#34661,#34662,#34663,#34664,#34665,#34666,#34667,#34668),
 .UNSPECIFIED.,.F.,.F.,(4,2,2,2,2,2,4),(0.00869408947528055,0.0191036740231402,
0.0270432080340005,0.0349827420448608,0.0429222760557212,0.0508618100665816,
0.0612713946144406),.UNSPECIFIED.);
#233=B_SPLINE_CURVE_WITH_KNOTS('',3,(#34683,#34684,#34685,#34686,#34687,
#34688,#34689,#34690,#34691,#34692,#34693,#34694,#34695,#34696),
 .UNSPECIFIED.,.F.,.F.,(4,2,2,2,2,2,4),(0.00869408947528055,0.0191036740231402,
0.0270432080340005,0.0349827420448608,0.0429222760557211,0.0508618100665814,
0.061271394614441),.UNSPECIFIED.);
#234=B_SPLINE_CURVE_WITH_KNOTS('',3,(#34724,#34725,#34726,#34727,#34728,
#34729,#34730,#34731,#34732,#34733,#34734,#34735,#34736,#34737),
 .UNSPECIFIED.,.F.,.F.,(4,2,2,2,2,2,4),(0.00869408947528073,0.0191036740231402,
0.0270432080340005,0.0349827420448608,0.0429222760557212,0.0508618100665817,
0.0612713946144409),.UNSPECIFIED.);
#235=B_SPLINE_CURVE_WITH_KNOTS('',3,(#34740,#34741,#34742,#34743,#34744,
#34745,#34746,#34747,#34748,#34749,#34750,#34751,#34752,#34753),
 .UNSPECIFIED.,.F.,.F.,(4,2,2,2,2,2,4),(0.00869408947528071,0.0191036740231402,
0.0270432080340005,0.0349827420448608,0.0429222760557211,0.0508618100665814,
0.0612713946144409),.UNSPECIFIED.);
#236=ELLIPSE('',#20061,0.0264106630927894,0.0146500000000133);
#237=ELLIPSE('',#20063,0.0264106630927895,0.0146500000000133);
#238=ELLIPSE('',#20064,0.0264106630927895,0.0146500000000133);
#239=ELLIPSE('',#20066,0.0264106630927894,0.0146500000000133);
#240=ELLIPSE('',#20069,0.0250585813644904,0.0139000000000133);
#241=ELLIPSE('',#20073,0.0250585813644904,0.0139000000000133);
#242=ELLIPSE('',#20076,0.0250585813644904,0.0139000000000133);
#243=ELLIPSE('',#20078,0.0250585813644904,0.0139000000000133);
#244=ELLIPSE('',#20089,0.0264106630927891,0.0146500000000128);
#245=ELLIPSE('',#20091,0.0264106630927891,0.0146500000000128);
#246=ELLIPSE('',#20092,0.0264106630927891,0.0146500000000128);
#247=ELLIPSE('',#20094,0.0264106630927891,0.0146500000000128);
#248=ELLIPSE('',#20097,0.0250585813644901,0.0139000000000128);
#249=ELLIPSE('',#20101,0.0250585813644901,0.0139000000000128);
#250=ELLIPSE('',#20104,0.0250585813644901,0.0139000000000128);
#251=ELLIPSE('',#20106,0.0250585813644901,0.0139000000000128);
#252=ELLIPSE('',#20117,0.0264106630927895,0.0146500000000133);
#253=ELLIPSE('',#20119,0.0264106630927894,0.0146500000000133);
#254=ELLIPSE('',#20120,0.0264106630927894,0.0146500000000133);
#255=ELLIPSE('',#20122,0.0264106630927895,0.0146500000000133);
#256=ELLIPSE('',#20125,0.0250585813644904,0.0139000000000133);
#257=ELLIPSE('',#20129,0.0250585813644904,0.0139000000000133);
#258=ELLIPSE('',#20132,0.0250585813644904,0.0139000000000133);
#259=ELLIPSE('',#20134,0.0250585813644904,0.0139000000000133);
#260=ELLIPSE('',#20145,0.0264106630927891,0.0146500000000128);
#261=ELLIPSE('',#20147,0.0264106630927891,0.0146500000000128);
#262=ELLIPSE('',#20148,0.0264106630927891,0.0146500000000128);
#263=ELLIPSE('',#20150,0.0264106630927891,0.0146500000000128);
#264=ELLIPSE('',#20153,0.0250585813644901,0.0139000000000128);
#265=ELLIPSE('',#20157,0.0250585813644901,0.0139000000000128);
#266=ELLIPSE('',#20160,0.0250585813644901,0.0139000000000128);
#267=ELLIPSE('',#20162,0.0250585813644901,0.0139000000000128);
#268=ELLIPSE('',#20173,0.0264106630927894,0.0146500000000133);
#269=ELLIPSE('',#20175,0.0264106630927895,0.0146500000000133);
#270=ELLIPSE('',#20176,0.0264106630927894,0.0146500000000133);
#271=ELLIPSE('',#20178,0.0264106630927894,0.0146500000000133);
#272=ELLIPSE('',#20181,0.0250585813644904,0.0139000000000133);
#273=ELLIPSE('',#20185,0.0250585813644904,0.0139000000000133);
#274=ELLIPSE('',#20188,0.0250585813644904,0.0139000000000133);
#275=ELLIPSE('',#20190,0.0250585813644904,0.0139000000000133);
#276=ELLIPSE('',#20201,0.0264106630927891,0.0146500000000128);
#277=ELLIPSE('',#20203,0.0264106630927891,0.0146500000000128);
#278=ELLIPSE('',#20204,0.0264106630927891,0.0146500000000128);
#279=ELLIPSE('',#20206,0.0264106630927891,0.0146500000000128);
#280=ELLIPSE('',#20209,0.0250585813644901,0.0139000000000128);
#281=ELLIPSE('',#20213,0.0250585813644901,0.0139000000000128);
#282=ELLIPSE('',#20216,0.0250585813644901,0.0139000000000128);
#283=ELLIPSE('',#20218,0.0250585813644901,0.0139000000000128);
#284=ELLIPSE('',#20229,0.0264106630927895,0.0146500000000133);
#285=ELLIPSE('',#20231,0.0264106630927894,0.0146500000000133);
#286=ELLIPSE('',#20232,0.0264106630927894,0.0146500000000133);
#287=ELLIPSE('',#20234,0.0264106630927895,0.0146500000000133);
#288=ELLIPSE('',#20237,0.0250585813644904,0.0139000000000133);
#289=ELLIPSE('',#20241,0.0250585813644904,0.0139000000000133);
#290=ELLIPSE('',#20244,0.0250585813644904,0.0139000000000133);
#291=ELLIPSE('',#20246,0.0250585813644904,0.0139000000000133);
#292=ELLIPSE('',#20257,0.0264106630927891,0.0146500000000128);
#293=ELLIPSE('',#20259,0.0264106630927891,0.0146500000000128);
#294=ELLIPSE('',#20260,0.0264106630927891,0.0146500000000128);
#295=ELLIPSE('',#20262,0.0264106630927891,0.0146500000000128);
#296=ELLIPSE('',#20265,0.0250585813644901,0.0139000000000128);
#297=ELLIPSE('',#20269,0.0250585813644901,0.0139000000000128);
#298=ELLIPSE('',#20272,0.0250585813644901,0.0139000000000128);
#299=ELLIPSE('',#20274,0.0250585813644901,0.0139000000000128);
#300=ELLIPSE('',#20594,0.114597376996511,0.00199999999998973);
#301=ELLIPSE('',#20596,0.00280406412973375,0.00199999999998973);
#302=ELLIPSE('',#20598,0.0352260556299788,0.0251250000000126);
#303=ELLIPSE('',#20600,0.0352260556299788,0.0251250000000126);
#304=ELLIPSE('',#20604,0.00280406412976774,0.00200000000001397);
#305=ELLIPSE('',#20606,0.114597376997899,0.00200000000001397);
#306=ELLIPSE('',#20609,0.114597376996524,0.00199999999998997);
#307=ELLIPSE('',#20611,0.00280406412973409,0.00199999999998997);
#308=ELLIPSE('',#20613,0.0352260556299805,0.0251250000000138);
#309=ELLIPSE('',#20615,0.0352260556299805,0.0251250000000138);
#310=ELLIPSE('',#20619,0.00280406412974482,0.00199999999999762);
#311=ELLIPSE('',#20621,0.114597376996964,0.00199999999999762);
#312=ELLIPSE('',#20624,0.114597376997842,0.00200000000001296);
#313=ELLIPSE('',#20626,0.00280406412976633,0.00200000000001296);
#314=ELLIPSE('',#20628,0.0352260556299806,0.0251250000000138);
#315=ELLIPSE('',#20630,0.0352260556299803,0.0251250000000138);
#316=ELLIPSE('',#20638,0.00280406412973409,0.00199999999998998);
#317=ELLIPSE('',#20639,0.114597376996526,0.00199999999998998);
#318=ELLIPSE('',#20642,0.0352260556300019,0.0251250000000291);
#319=ELLIPSE('',#20645,0.0352260556300016,0.0251250000000291);
#320=ELLIPSE('',#20648,0.114597376997269,0.00200000000000295);
#321=ELLIPSE('',#20649,0.00280406412975229,0.00200000000000295);
#322=ELLIPSE('',#20653,0.114597376996301,0.00199999999998605);
#323=ELLIPSE('',#20654,0.00280406412972858,0.00199999999998605);
#324=ELLIPSE('',#20968,0.00280406412975229,0.00200000000000295);
#325=ELLIPSE('',#20969,0.114597376997271,0.00200000000000295);
#326=ELLIPSE('',#20972,0.0352260556300016,0.0251250000000291);
#327=ELLIPSE('',#20974,0.0352260556300019,0.0251250000000291);
#328=ELLIPSE('',#20977,0.00280406412976774,0.00200000000001397);
#329=ELLIPSE('',#20978,0.114597376997902,0.00200000000001397);
#330=ELLIPSE('',#20981,0.0352260556299788,0.0251250000000126);
#331=ELLIPSE('',#20983,0.0352260556299788,0.0251250000000126);
#332=ELLIPSE('',#20986,0.00280406412974482,0.00199999999999762);
#333=ELLIPSE('',#20987,0.114597376996966,0.00199999999999762);
#334=ELLIPSE('',#20990,0.0352260556299805,0.0251250000000138);
#335=ELLIPSE('',#20992,0.0352260556299805,0.0251250000000138);
#336=ELLIPSE('',#20995,0.00280406412972858,0.00199999999998605);
#337=ELLIPSE('',#20996,0.114597376996303,0.00199999999998605);
#338=ELLIPSE('',#20999,0.0352260556299806,0.0251250000000138);
#339=ELLIPSE('',#21001,0.0352260556299803,0.0251250000000138);
#340=ELLIPSE('',#21004,0.114597376996528,0.00199999999998998);
#341=ELLIPSE('',#21005,0.00280406412973409,0.00199999999998998);
#342=ELLIPSE('',#21008,0.114597376996513,0.00199999999998973);
#343=ELLIPSE('',#21009,0.00280406412973375,0.00199999999998973);
#344=ELLIPSE('',#21012,0.114597376996527,0.00199999999998997);
#345=ELLIPSE('',#21013,0.00280406412973409,0.00199999999998997);
#346=ELLIPSE('',#21016,0.114597376997844,0.00200000000001296);
#347=ELLIPSE('',#21017,0.00280406412976633,0.00200000000001296);
#348=SHAPE_REPRESENTATION_RELATIONSHIP('SRR','None',#34985,#381);
#349=SHAPE_REPRESENTATION_RELATIONSHIP('SRR','None',#34986,#382);
#350=SHAPE_REPRESENTATION_RELATIONSHIP('SRR','None',#34987,#383);
#351=SHAPE_REPRESENTATION_RELATIONSHIP('SRR','None',#34988,#384);
#352=SHAPE_REPRESENTATION_RELATIONSHIP('SRR','None',#34989,#385);
#353=SHAPE_REPRESENTATION_RELATIONSHIP('SRR','None',#34990,#386);
#354=SHAPE_REPRESENTATION_RELATIONSHIP('SRR','None',#34991,#387);
#355=SHAPE_REPRESENTATION_RELATIONSHIP('SRR','None',#34992,#388);
#356=SHAPE_REPRESENTATION_RELATIONSHIP('SRR','None',#34993,#389);
#357=SHAPE_REPRESENTATION_RELATIONSHIP('SRR','None',#34994,#390);
#358=SHAPE_REPRESENTATION_RELATIONSHIP('SRR','None',#34995,#391);
#359=SHAPE_REPRESENTATION_RELATIONSHIP('SRR','None',#34996,#392);
#360=SHAPE_REPRESENTATION_RELATIONSHIP('SRR','None',#34997,#393);
#361=SHAPE_REPRESENTATION_RELATIONSHIP('SRR','None',#34998,#394);
#362=SHAPE_REPRESENTATION_RELATIONSHIP('SRR','None',#34999,#395);
#363=SHAPE_REPRESENTATION_RELATIONSHIP('SRR','None',#35000,#396);
#364=SHAPE_REPRESENTATION_RELATIONSHIP('SRR','None',#35001,#397);
#365=SHAPE_REPRESENTATION_RELATIONSHIP('SRR','None',#35002,#398);
#366=SHAPE_REPRESENTATION_RELATIONSHIP('SRR','None',#35003,#399);
#367=SHAPE_REPRESENTATION_RELATIONSHIP('SRR','None',#35004,#400);
#368=SHAPE_REPRESENTATION_RELATIONSHIP('SRR','None',#35005,#401);
#369=SHAPE_REPRESENTATION_RELATIONSHIP('SRR','None',#35006,#402);
#370=SHAPE_REPRESENTATION_RELATIONSHIP('SRR','None',#35007,#403);
#371=SHAPE_REPRESENTATION_RELATIONSHIP('SRR','None',#35008,#404);
#372=SHAPE_REPRESENTATION_RELATIONSHIP('SRR','None',#35009,#405);
#373=SHAPE_REPRESENTATION_RELATIONSHIP('SRR','None',#35010,#406);
#374=SHAPE_REPRESENTATION_RELATIONSHIP('SRR','None',#35011,#407);
#375=SHAPE_REPRESENTATION_RELATIONSHIP('SRR','None',#35012,#408);
#376=SHAPE_REPRESENTATION_RELATIONSHIP('SRR','None',#35013,#409);
#377=SHAPE_REPRESENTATION_RELATIONSHIP('SRR','None',#35014,#410);
#378=SHAPE_REPRESENTATION_RELATIONSHIP('SRR','None',#35015,#411);
#379=SHAPE_REPRESENTATION_RELATIONSHIP('SRR','None',#35016,#412);
#380=SHAPE_REPRESENTATION_RELATIONSHIP('SRR','None',#35017,#413);
#381=ADVANCED_BREP_SHAPE_REPRESENTATION('',(#447),#34843);
#382=ADVANCED_BREP_SHAPE_REPRESENTATION('',(#448),#34844);
#383=ADVANCED_BREP_SHAPE_REPRESENTATION('',(#449),#34845);
#384=ADVANCED_BREP_SHAPE_REPRESENTATION('',(#450),#34846);
#385=ADVANCED_BREP_SHAPE_REPRESENTATION('',(#451),#34847);
#386=ADVANCED_BREP_SHAPE_REPRESENTATION('',(#452),#34848);
#387=ADVANCED_BREP_SHAPE_REPRESENTATION('',(#453),#34849);
#388=ADVANCED_BREP_SHAPE_REPRESENTATION('',(#454),#34850);
#389=ADVANCED_BREP_SHAPE_REPRESENTATION('',(#455),#34851);
#390=ADVANCED_BREP_SHAPE_REPRESENTATION('',(#456),#34852);
#391=ADVANCED_BREP_SHAPE_REPRESENTATION('',(#457),#34853);
#392=ADVANCED_BREP_SHAPE_REPRESENTATION('',(#458),#34854);
#393=ADVANCED_BREP_SHAPE_REPRESENTATION('',(#459),#34855);
#394=ADVANCED_BREP_SHAPE_REPRESENTATION('',(#460),#34856);
#395=ADVANCED_BREP_SHAPE_REPRESENTATION('',(#461),#34857);
#396=ADVANCED_BREP_SHAPE_REPRESENTATION('',(#462),#34858);
#397=ADVANCED_BREP_SHAPE_REPRESENTATION('',(#463),#34859);
#398=ADVANCED_BREP_SHAPE_REPRESENTATION('',(#464),#34860);
#399=ADVANCED_BREP_SHAPE_REPRESENTATION('',(#465),#34861);
#400=ADVANCED_BREP_SHAPE_REPRESENTATION('',(#466),#34862);
#401=ADVANCED_BREP_SHAPE_REPRESENTATION('',(#467),#34863);
#402=ADVANCED_BREP_SHAPE_REPRESENTATION('',(#468),#34864);
#403=ADVANCED_BREP_SHAPE_REPRESENTATION('',(#469),#34865);
#404=ADVANCED_BREP_SHAPE_REPRESENTATION('',(#470),#34866);
#405=ADVANCED_BREP_SHAPE_REPRESENTATION('',(#471),#34867);
#406=ADVANCED_BREP_SHAPE_REPRESENTATION('',(#472),#34868);
#407=ADVANCED_BREP_SHAPE_REPRESENTATION('',(#473),#34869);
#408=ADVANCED_BREP_SHAPE_REPRESENTATION('',(#474),#34870);
#409=ADVANCED_BREP_SHAPE_REPRESENTATION('',(#475),#34871);
#410=ADVANCED_BREP_SHAPE_REPRESENTATION('',(#476),#34872);
#411=ADVANCED_BREP_SHAPE_REPRESENTATION('',(#477),#34873);
#412=ADVANCED_BREP_SHAPE_REPRESENTATION('',(#478),#34874);
#413=ADVANCED_BREP_SHAPE_REPRESENTATION('',(#479),#34875);
#414=STYLED_ITEM('',(#35159),#447);
#415=STYLED_ITEM('',(#35160),#448);
#416=STYLED_ITEM('',(#35161),#449);
#417=STYLED_ITEM('',(#35162),#450);
#418=STYLED_ITEM('',(#35163),#451);
#419=STYLED_ITEM('',(#35159),#452);
#420=STYLED_ITEM('',(#35161),#453);
#421=STYLED_ITEM('',(#35164),#454);
#422=STYLED_ITEM('',(#35165),#455);
#423=STYLED_ITEM('',(#35159),#456);
#424=STYLED_ITEM('',(#35166),#457);
#425=STYLED_ITEM('',(#35162),#458);
#426=STYLED_ITEM('',(#35163),#459);
#427=STYLED_ITEM('',(#35159),#460);
#428=STYLED_ITEM('',(#35160),#461);
#429=STYLED_ITEM('',(#35161),#462);
#430=STYLED_ITEM('',(#35164),#463);
#431=STYLED_ITEM('',(#35162),#464);
#432=STYLED_ITEM('',(#35159),#465);
#433=STYLED_ITEM('',(#35166),#466);
#434=STYLED_ITEM('',(#35161),#467);
#435=STYLED_ITEM('',(#35163),#468);
#436=STYLED_ITEM('',(#35165),#469);
#437=STYLED_ITEM('',(#35159),#470);
#438=STYLED_ITEM('',(#35166),#471);
#439=STYLED_ITEM('',(#35160),#472);
#440=STYLED_ITEM('',(#35161),#473);
#441=STYLED_ITEM('',(#35164),#474);
#442=STYLED_ITEM('',(#35162),#475);
#443=STYLED_ITEM('',(#35163),#476);
#444=STYLED_ITEM('',(#35165),#477);
#445=STYLED_ITEM('',(#35159),#478);
#446=STYLED_ITEM('',(#35164),#479);
#447=MANIFOLD_SOLID_BREP('Dowel Pin 5x16 Long 1',#19554);
#448=MANIFOLD_SOLID_BREP('Motor Stator Face 1',#19555);
#449=MANIFOLD_SOLID_BREP('Motor Plastic Spacer Right',#19556);
#450=MANIFOLD_SOLID_BREP('Motor Plastic Cover 1',#19557);
#451=MANIFOLD_SOLID_BREP('Motor Shaft 1',#19558);
#452=MANIFOLD_SOLID_BREP('Motor Base Cap',#19559);
#453=MANIFOLD_SOLID_BREP('Dowel Pin 5x16 1',#19560);
#454=MANIFOLD_SOLID_BREP('Socket Screw 1',#19561);
#455=MANIFOLD_SOLID_BREP('Socket Screw 2',#19562);
#456=MANIFOLD_SOLID_BREP('External Shaft Retaining Ring Clip',#19563);
#457=MANIFOLD_SOLID_BREP('Motor Stator Face 2',#19564);
#458=MANIFOLD_SOLID_BREP('Motor Top Cap',#19565);
#459=MANIFOLD_SOLID_BREP('Motor Stator Face 3',#19566);
#460=MANIFOLD_SOLID_BREP('Motor Shaft 2',#19567);
#461=MANIFOLD_SOLID_BREP('Motor Plastic Protector',#19568);
#462=MANIFOLD_SOLID_BREP('Motor PCB',#19569);
#463=MANIFOLD_SOLID_BREP('Socket Screw 3',#19570);
#464=MANIFOLD_SOLID_BREP('Motor Stator Face 4',#19571);
#465=MANIFOLD_SOLID_BREP('Motor Plastic Spacer Left',#19572);
#466=MANIFOLD_SOLID_BREP('Socket Screw 4',#19573);
#467=MANIFOLD_SOLID_BREP('Motor Shaft 3',#19574);
#468=MANIFOLD_SOLID_BREP('Dowel Pin 5x16 2',#19575);
#469=MANIFOLD_SOLID_BREP('Motor Stator Face 5',#19576);
#470=MANIFOLD_SOLID_BREP('Socket Screw 5',#19577);
#471=MANIFOLD_SOLID_BREP('Motor Central Spacer',#19578);
#472=MANIFOLD_SOLID_BREP('Motor Stator Face 6',#19579);
#473=MANIFOLD_SOLID_BREP('Socket Screw 6',#19580);
#474=MANIFOLD_SOLID_BREP('Motor Shaft 4',#19581);
#475=MANIFOLD_SOLID_BREP('Motor Stator Face 7',#19582);
#476=MANIFOLD_SOLID_BREP('Motor Stator Face 8',#19583);
#477=MANIFOLD_SOLID_BREP('Dowel Pin 5x16 Long 2',#19584);
#478=MANIFOLD_SOLID_BREP('Socket Screw 7',#19585);
#479=MANIFOLD_SOLID_BREP('Pan Head Screw M3x25 1',#19586);
#480=FACE_BOUND('',#5841,.T.);
#481=FACE_BOUND('',#5844,.T.);
#482=FACE_BOUND('',#5883,.T.);
#483=FACE_BOUND('',#5887,.T.);
#484=FACE_BOUND('',#5889,.T.);
#485=FACE_BOUND('',#5904,.T.);
#486=FACE_BOUND('',#5919,.T.);
#487=FACE_BOUND('',#5934,.T.);
#488=FACE_BOUND('',#5949,.T.);
#489=FACE_BOUND('',#5964,.T.);
#490=FACE_BOUND('',#5979,.T.);
#491=FACE_BOUND('',#5994,.T.);
#492=FACE_BOUND('',#6009,.T.);
#493=FACE_BOUND('',#6018,.T.);
#494=FACE_BOUND('',#6020,.T.);
#495=FACE_BOUND('',#6022,.T.);
#496=FACE_BOUND('',#6024,.T.);
#497=FACE_BOUND('',#6026,.T.);
#498=FACE_BOUND('',#6028,.T.);
#499=FACE_BOUND('',#6030,.T.);
#500=FACE_BOUND('',#6032,.T.);
#501=FACE_BOUND('',#6091,.T.);
#502=FACE_BOUND('',#6138,.T.);
#503=FACE_BOUND('',#6175,.T.);
#504=FACE_BOUND('',#6184,.T.);
#505=FACE_BOUND('',#6185,.T.);
#506=FACE_BOUND('',#6186,.T.);
#507=FACE_BOUND('',#6187,.T.);
#508=FACE_BOUND('',#6224,.T.);
#509=FACE_BOUND('',#6229,.T.);
#510=FACE_BOUND('',#6232,.T.);
#511=FACE_BOUND('',#6235,.T.);
#512=FACE_BOUND('',#6238,.T.);
#513=FACE_BOUND('',#6241,.T.);
#514=FACE_BOUND('',#6242,.T.);
#515=FACE_BOUND('',#6245,.T.);
#516=FACE_BOUND('',#6247,.T.);
#517=FACE_BOUND('',#6255,.T.);
#518=FACE_BOUND('',#6258,.T.);
#519=FACE_BOUND('',#6354,.T.);
#520=FACE_BOUND('',#6355,.T.);
#521=FACE_BOUND('',#6356,.T.);
#522=FACE_BOUND('',#6357,.T.);
#523=FACE_BOUND('',#6358,.T.);
#524=FACE_BOUND('',#6361,.T.);
#525=FACE_BOUND('',#6362,.T.);
#526=FACE_BOUND('',#6363,.T.);
#527=FACE_BOUND('',#6364,.T.);
#528=FACE_BOUND('',#6365,.T.);
#529=FACE_BOUND('',#6379,.T.);
#530=FACE_BOUND('',#6383,.T.);
#531=FACE_BOUND('',#6389,.T.);
#532=FACE_BOUND('',#6392,.T.);
#533=FACE_BOUND('',#6402,.T.);
#534=FACE_BOUND('',#6448,.T.);
#535=FACE_BOUND('',#6450,.T.);
#536=FACE_BOUND('',#6495,.T.);
#537=FACE_BOUND('',#6496,.T.);
#538=FACE_BOUND('',#6497,.T.);
#539=FACE_BOUND('',#6498,.T.);
#540=FACE_BOUND('',#6499,.T.);
#541=FACE_BOUND('',#6500,.T.);
#542=FACE_BOUND('',#6501,.T.);
#543=FACE_BOUND('',#6502,.T.);
#544=FACE_BOUND('',#6503,.T.);
#545=FACE_BOUND('',#6504,.T.);
#546=FACE_BOUND('',#6506,.T.);
#547=FACE_BOUND('',#6507,.T.);
#548=FACE_BOUND('',#6508,.T.);
#549=FACE_BOUND('',#6509,.T.);
#550=FACE_BOUND('',#6510,.T.);
#551=FACE_BOUND('',#6511,.T.);
#552=FACE_BOUND('',#6512,.T.);
#553=FACE_BOUND('',#6513,.T.);
#554=FACE_BOUND('',#6514,.T.);
#555=FACE_BOUND('',#6515,.T.);
#556=FACE_BOUND('',#6562,.T.);
#557=FACE_BOUND('',#6566,.T.);
#558=FACE_BOUND('',#6621,.T.);
#559=FACE_BOUND('',#6668,.T.);
#560=FACE_BOUND('',#6674,.T.);
#561=FACE_BOUND('',#6677,.T.);
#562=FACE_BOUND('',#6740,.T.);
#563=FACE_BOUND('',#6741,.T.);
#564=FACE_BOUND('',#6742,.T.);
#565=FACE_BOUND('',#6743,.T.);
#566=FACE_BOUND('',#6744,.T.);
#567=FACE_BOUND('',#6759,.T.);
#568=FACE_BOUND('',#6760,.T.);
#569=FACE_BOUND('',#6761,.T.);
#570=FACE_BOUND('',#6762,.T.);
#571=FACE_BOUND('',#6763,.T.);
#572=FACE_BOUND('',#6831,.T.);
#573=FACE_BOUND('',#6832,.T.);
#574=FACE_BOUND('',#6833,.T.);
#575=FACE_BOUND('',#6834,.T.);
#576=FACE_BOUND('',#6835,.T.);
#577=FACE_BOUND('',#6836,.T.);
#578=FACE_BOUND('',#6858,.T.);
#579=FACE_BOUND('',#6859,.T.);
#580=FACE_BOUND('',#6860,.T.);
#581=FACE_BOUND('',#6861,.T.);
#582=FACE_BOUND('',#6862,.T.);
#583=FACE_BOUND('',#6863,.T.);
#584=FACE_BOUND('',#6869,.T.);
#585=FACE_BOUND('',#6871,.T.);
#586=FACE_BOUND('',#6947,.T.);
#587=FACE_BOUND('',#6950,.T.);
#588=FACE_BOUND('',#6974,.T.);
#589=FACE_BOUND('',#6991,.T.);
#590=PLANE('',#19961);
#591=PLANE('',#19966);
#592=PLANE('',#19979);
#593=PLANE('',#19989);
#594=PLANE('',#19999);
#595=PLANE('',#20009);
#596=PLANE('',#20019);
#597=PLANE('',#20020);
#598=PLANE('',#20021);
#599=PLANE('',#20022);
#600=PLANE('',#20023);
#601=PLANE('',#20030);
#602=PLANE('',#20040);
#603=PLANE('',#20045);
#604=PLANE('',#20048);
#605=PLANE('',#20049);
#606=PLANE('',#20051);
#607=PLANE('',#20058);
#608=PLANE('',#20067);
#609=PLANE('',#20068);
#610=PLANE('',#20070);
#611=PLANE('',#20072);
#612=PLANE('',#20074);
#613=PLANE('',#20075);
#614=PLANE('',#20080);
#615=PLANE('',#20081);
#616=PLANE('',#20082);
#617=PLANE('',#20087);
#618=PLANE('',#20095);
#619=PLANE('',#20096);
#620=PLANE('',#20098);
#621=PLANE('',#20100);
#622=PLANE('',#20102);
#623=PLANE('',#20103);
#624=PLANE('',#20108);
#625=PLANE('',#20109);
#626=PLANE('',#20110);
#627=PLANE('',#20115);
#628=PLANE('',#20123);
#629=PLANE('',#20124);
#630=PLANE('',#20126);
#631=PLANE('',#20128);
#632=PLANE('',#20130);
#633=PLANE('',#20131);
#634=PLANE('',#20136);
#635=PLANE('',#20137);
#636=PLANE('',#20138);
#637=PLANE('',#20143);
#638=PLANE('',#20151);
#639=PLANE('',#20152);
#640=PLANE('',#20154);
#641=PLANE('',#20156);
#642=PLANE('',#20158);
#643=PLANE('',#20159);
#644=PLANE('',#20164);
#645=PLANE('',#20165);
#646=PLANE('',#20166);
#647=PLANE('',#20171);
#648=PLANE('',#20179);
#649=PLANE('',#20180);
#650=PLANE('',#20182);
#651=PLANE('',#20184);
#652=PLANE('',#20186);
#653=PLANE('',#20187);
#654=PLANE('',#20192);
#655=PLANE('',#20193);
#656=PLANE('',#20194);
#657=PLANE('',#20199);
#658=PLANE('',#20207);
#659=PLANE('',#20208);
#660=PLANE('',#20210);
#661=PLANE('',#20212);
#662=PLANE('',#20214);
#663=PLANE('',#20215);
#664=PLANE('',#20220);
#665=PLANE('',#20221);
#666=PLANE('',#20222);
#667=PLANE('',#20227);
#668=PLANE('',#20235);
#669=PLANE('',#20236);
#670=PLANE('',#20238);
#671=PLANE('',#20240);
#672=PLANE('',#20242);
#673=PLANE('',#20243);
#674=PLANE('',#20248);
#675=PLANE('',#20249);
#676=PLANE('',#20250);
#677=PLANE('',#20255);
#678=PLANE('',#20263);
#679=PLANE('',#20264);
#680=PLANE('',#20266);
#681=PLANE('',#20268);
#682=PLANE('',#20270);
#683=PLANE('',#20271);
#684=PLANE('',#20276);
#685=PLANE('',#20277);
#686=PLANE('',#20278);
#687=PLANE('',#20285);
#688=PLANE('',#20286);
#689=PLANE('',#20287);
#690=PLANE('',#20288);
#691=PLANE('',#20289);
#692=PLANE('',#20290);
#693=PLANE('',#20291);
#694=PLANE('',#20292);
#695=PLANE('',#20293);
#696=PLANE('',#20294);
#697=PLANE('',#20295);
#698=PLANE('',#20296);
#699=PLANE('',#20297);
#700=PLANE('',#20298);
#701=PLANE('',#20299);
#702=PLANE('',#20300);
#703=PLANE('',#20301);
#704=PLANE('',#20302);
#705=PLANE('',#20303);
#706=PLANE('',#20304);
#707=PLANE('',#20305);
#708=PLANE('',#20306);
#709=PLANE('',#20307);
#710=PLANE('',#20308);
#711=PLANE('',#20309);
#712=PLANE('',#20310);
#713=PLANE('',#20311);
#714=PLANE('',#20312);
#715=PLANE('',#20313);
#716=PLANE('',#20314);
#717=PLANE('',#20448);
#718=PLANE('',#20586);
#719=PLANE('',#20592);
#720=PLANE('',#20607);
#721=PLANE('',#20622);
#722=PLANE('',#20633);
#723=PLANE('',#20634);
#724=PLANE('',#20635);
#725=PLANE('',#20636);
#726=PLANE('',#20655);
#727=PLANE('',#20656);
#728=PLANE('',#20657);
#729=PLANE('',#20663);
#730=PLANE('',#20664);
#731=PLANE('',#20670);
#732=PLANE('',#20671);
#733=PLANE('',#20677);
#734=PLANE('',#20678);
#735=PLANE('',#20679);
#736=PLANE('',#20680);
#737=PLANE('',#20681);
#738=PLANE('',#20699);
#739=PLANE('',#20700);
#740=PLANE('',#20708);
#741=PLANE('',#20709);
#742=PLANE('',#20710);
#743=PLANE('',#20711);
#744=PLANE('',#20712);
#745=PLANE('',#20713);
#746=PLANE('',#20714);
#747=PLANE('',#20718);
#748=PLANE('',#20722);
#749=PLANE('',#20726);
#750=PLANE('',#20730);
#751=PLANE('',#20731);
#752=PLANE('',#20732);
#753=PLANE('',#20733);
#754=PLANE('',#20736);
#755=PLANE('',#20737);
#756=PLANE('',#20741);
#757=PLANE('',#20745);
#758=PLANE('',#20749);
#759=PLANE('',#20750);
#760=PLANE('',#20751);
#761=PLANE('',#20755);
#762=PLANE('',#20756);
#763=PLANE('',#20757);
#764=PLANE('',#20761);
#765=PLANE('',#20770);
#766=PLANE('',#20773);
#767=PLANE('',#20776);
#768=PLANE('',#20779);
#769=PLANE('',#20782);
#770=PLANE('',#20786);
#771=PLANE('',#20787);
#772=PLANE('',#20788);
#773=PLANE('',#20789);
#774=PLANE('',#20790);
#775=PLANE('',#20791);
#776=PLANE('',#20801);
#777=PLANE('',#20806);
#778=PLANE('',#20810);
#779=PLANE('',#20811);
#780=PLANE('',#20815);
#781=PLANE('',#20816);
#782=PLANE('',#20817);
#783=PLANE('',#20818);
#784=PLANE('',#20819);
#785=PLANE('',#20820);
#786=PLANE('',#20822);
#787=PLANE('',#20823);
#788=PLANE('',#20827);
#789=PLANE('',#20828);
#790=PLANE('',#20829);
#791=PLANE('',#20830);
#792=PLANE('',#20831);
#793=PLANE('',#20832);
#794=PLANE('',#20840);
#795=PLANE('',#20847);
#796=PLANE('',#20857);
#797=PLANE('',#20861);
#798=PLANE('',#20871);
#799=PLANE('',#20878);
#800=PLANE('',#20882);
#801=PLANE('',#20883);
#802=PLANE('',#20894);
#803=PLANE('',#20904);
#804=PLANE('',#20914);
#805=PLANE('',#20924);
#806=PLANE('',#20934);
#807=PLANE('',#20935);
#808=PLANE('',#20936);
#809=PLANE('',#20937);
#810=PLANE('',#20938);
#811=PLANE('',#20945);
#812=PLANE('',#20955);
#813=PLANE('',#20958);
#814=PLANE('',#20961);
#815=PLANE('',#20964);
#816=PLANE('',#21018);
#817=PLANE('',#21019);
#818=PLANE('',#21020);
#819=PLANE('',#21021);
#820=PLANE('',#21022);
#821=PLANE('',#21023);
#822=PLANE('',#21028);
#823=PLANE('',#21029);
#824=PLANE('',#21035);
#825=PLANE('',#21036);
#826=PLANE('',#21037);
#827=PLANE('',#21038);
#828=PLANE('',#21039);
#829=PLANE('',#21040);
#830=PLANE('',#21041);
#831=PLANE('',#21042);
#832=PLANE('',#21043);
#833=PLANE('',#21044);
#834=PLANE('',#21045);
#835=PLANE('',#21046);
#836=PLANE('',#21047);
#837=PLANE('',#21049);
#838=PLANE('',#21054);
#839=PLANE('',#21064);
#840=PLANE('',#21069);
#841=PLANE('',#21083);
#842=PLANE('',#21084);
#843=PLANE('',#21085);
#844=PLANE('',#21086);
#845=PLANE('',#21087);
#846=PLANE('',#21088);
#847=PLANE('',#21099);
#848=PLANE('',#21109);
#849=PLANE('',#21119);
#850=PLANE('',#21129);
#851=PLANE('',#21139);
#852=PLANE('',#21140);
#853=PLANE('',#21141);
#854=PLANE('',#21142);
#855=PLANE('',#21143);
#856=PLANE('',#21150);
#857=PLANE('',#21160);
#858=PLANE('',#21163);
#859=PLANE('',#21166);
#860=PLANE('',#21169);
#861=PLANE('',#21181);
#862=PLANE('',#21183);
#863=PLANE('',#21187);
#864=PLANE('',#21188);
#865=PLANE('',#21194);
#866=PLANE('',#21195);
#867=PLANE('',#21197);
#868=PLANE('',#21198);
#869=PLANE('',#21199);
#870=PLANE('',#21200);
#871=PLANE('',#21201);
#872=PLANE('',#21202);
#873=PLANE('',#21204);
#874=PLANE('',#21205);
#875=PLANE('',#21206);
#876=PLANE('',#21207);
#877=PLANE('',#21208);
#878=PLANE('',#21211);
#879=PLANE('',#21212);
#880=PLANE('',#21213);
#881=PLANE('',#21214);
#882=PLANE('',#21246);
#883=PLANE('',#21247);
#884=PLANE('',#21248);
#885=PLANE('',#21249);
#886=PLANE('',#21250);
#887=PLANE('',#21251);
#888=PLANE('',#21252);
#889=PLANE('',#21256);
#890=PLANE('',#21257);
#891=PLANE('',#21258);
#892=PLANE('',#21259);
#893=PLANE('',#21261);
#894=PLANE('',#21262);
#895=PLANE('',#21266);
#896=PLANE('',#21267);
#897=PLANE('',#21268);
#898=PLANE('',#21269);
#899=PLANE('',#21270);
#900=PLANE('',#21271);
#901=PLANE('',#21282);
#902=PLANE('',#21292);
#903=PLANE('',#21302);
#904=PLANE('',#21312);
#905=PLANE('',#21322);
#906=PLANE('',#21323);
#907=PLANE('',#21324);
#908=PLANE('',#21325);
#909=PLANE('',#21326);
#910=PLANE('',#21333);
#911=PLANE('',#21343);
#912=PLANE('',#21348);
#913=PLANE('',#21351);
#914=PLANE('',#21352);
#915=PLANE('',#21354);
#916=PLANE('',#21361);
#917=PLANE('',#21363);
#918=PLANE('',#21364);
#919=PLANE('',#21365);
#920=PLANE('',#21369);
#921=PLANE('',#21370);
#922=PLANE('',#21371);
#923=PLANE('',#21372);
#924=PLANE('',#21373);
#925=PLANE('',#21507);
#926=PLANE('',#21645);
#927=PLANE('',#21659);
#928=PLANE('',#21664);
#929=PLANE('',#21677);
#930=PLANE('',#21687);
#931=PLANE('',#21697);
#932=PLANE('',#21707);
#933=PLANE('',#21717);
#934=PLANE('',#21718);
#935=PLANE('',#21719);
#936=PLANE('',#21720);
#937=PLANE('',#21721);
#938=PLANE('',#21728);
#939=PLANE('',#21738);
#940=PLANE('',#21741);
#941=PLANE('',#21744);
#942=PLANE('',#21747);
#943=PLANE('',#21749);
#944=PLANE('',#21750);
#945=PLANE('',#21751);
#946=PLANE('',#21752);
#947=PLANE('',#21756);
#948=PLANE('',#21757);
#949=PLANE('',#21758);
#950=PLANE('',#21759);
#951=PLANE('',#21764);
#952=PLANE('',#21774);
#953=PLANE('',#21784);
#954=PLANE('',#21794);
#955=PLANE('',#21798);
#956=PLANE('',#21814);
#957=PLANE('',#21815);
#958=PLANE('',#21816);
#959=PLANE('',#21817);
#960=PLANE('',#21818);
#961=PLANE('',#21819);
#962=PLANE('',#21820);
#963=PLANE('',#21821);
#964=PLANE('',#21822);
#965=PLANE('',#21833);
#966=PLANE('',#21843);
#967=PLANE('',#21853);
#968=PLANE('',#21863);
#969=PLANE('',#21873);
#970=PLANE('',#21874);
#971=PLANE('',#21875);
#972=PLANE('',#21876);
#973=PLANE('',#21877);
#974=PLANE('',#21884);
#975=PLANE('',#21894);
#976=PLANE('',#21899);
#977=PLANE('',#21902);
#978=PLANE('',#21903);
#979=PLANE('',#21905);
#980=PLANE('',#21906);
#981=PLANE('',#21907);
#982=PLANE('',#21908);
#983=PLANE('',#21909);
#984=PLANE('',#21910);
#985=PLANE('',#21911);
#986=PLANE('',#21912);
#987=PLANE('',#21913);
#988=PLANE('',#21914);
#989=PLANE('',#21915);
#990=PLANE('',#21916);
#991=PLANE('',#21917);
#992=PLANE('',#21918);
#993=PLANE('',#21919);
#994=PLANE('',#21920);
#995=PLANE('',#21921);
#996=PLANE('',#21922);
#997=PLANE('',#21923);
#998=PLANE('',#21924);
#999=PLANE('',#21925);
#1000=PLANE('',#21926);
#1001=PLANE('',#21927);
#1002=PLANE('',#21928);
#1003=PLANE('',#21929);
#1004=PLANE('',#21930);
#1005=PLANE('',#21931);
#1006=PLANE('',#21932);
#1007=PLANE('',#21933);
#1008=PLANE('',#21934);
#1009=PLANE('',#21935);
#1010=PLANE('',#21936);
#1011=PLANE('',#21937);
#1012=PLANE('',#21938);
#1013=PLANE('',#21939);
#1014=PLANE('',#21940);
#1015=PLANE('',#21941);
#1016=PLANE('',#21942);
#1017=PLANE('',#21943);
#1018=PLANE('',#21944);
#1019=PLANE('',#21945);
#1020=PLANE('',#21946);
#1021=PLANE('',#21947);
#1022=PLANE('',#21948);
#1023=PLANE('',#21949);
#1024=PLANE('',#21950);
#1025=PLANE('',#21951);
#1026=PLANE('',#21952);
#1027=PLANE('',#21953);
#1028=PLANE('',#21954);
#1029=PLANE('',#21955);
#1030=PLANE('',#21956);
#1031=PLANE('',#21957);
#1032=PLANE('',#21958);
#1033=PLANE('',#21966);
#1034=PLANE('',#21967);
#1035=PLANE('',#21978);
#1036=PLANE('',#21988);
#1037=PLANE('',#21998);
#1038=PLANE('',#22008);
#1039=PLANE('',#22018);
#1040=PLANE('',#22019);
#1041=PLANE('',#22020);
#1042=PLANE('',#22021);
#1043=PLANE('',#22022);
#1044=PLANE('',#22029);
#1045=PLANE('',#22039);
#1046=PLANE('',#22042);
#1047=PLANE('',#22045);
#1048=PLANE('',#22048);
#1049=PLANE('',#22059);
#1050=PLANE('',#22069);
#1051=PLANE('',#22079);
#1052=PLANE('',#22089);
#1053=PLANE('',#22099);
#1054=PLANE('',#22100);
#1055=PLANE('',#22101);
#1056=PLANE('',#22102);
#1057=PLANE('',#22103);
#1058=PLANE('',#22110);
#1059=PLANE('',#22120);
#1060=PLANE('',#22123);
#1061=PLANE('',#22126);
#1062=PLANE('',#22129);
#1063=PLANE('',#22139);
#1064=PLANE('',#22144);
#1065=PLANE('',#22148);
#1066=PLANE('',#22149);
#1067=PLANE('',#22153);
#1068=PLANE('',#22154);
#1069=PLANE('',#22155);
#1070=PLANE('',#22156);
#1071=PLANE('',#22157);
#1072=PLANE('',#22158);
#1073=PLANE('',#22166);
#1074=PLANE('',#22205);
#1075=PLANE('',#22206);
#1076=PLANE('',#22208);
#1077=PLANE('',#22209);
#1078=PLANE('',#22210);
#1079=PLANE('',#22211);
#1080=PLANE('',#22212);
#1081=PLANE('',#22215);
#1082=PLANE('',#22220);
#1083=LINE('',#28483,#2682);
#1084=LINE('',#28498,#2683);
#1085=LINE('',#28505,#2684);
#1086=LINE('',#28508,#2685);
#1087=LINE('',#28513,#2686);
#1088=LINE('',#28519,#2687);
#1089=LINE('',#28523,#2688);
#1090=LINE('',#28525,#2689);
#1091=LINE('',#28526,#2690);
#1092=LINE('',#28532,#2691);
#1093=LINE('',#28535,#2692);
#1094=LINE('',#28540,#2693);
#1095=LINE('',#28546,#2694);
#1096=LINE('',#28550,#2695);
#1097=LINE('',#28552,#2696);
#1098=LINE('',#28553,#2697);
#1099=LINE('',#28559,#2698);
#1100=LINE('',#28562,#2699);
#1101=LINE('',#28567,#2700);
#1102=LINE('',#28573,#2701);
#1103=LINE('',#28577,#2702);
#1104=LINE('',#28579,#2703);
#1105=LINE('',#28580,#2704);
#1106=LINE('',#28586,#2705);
#1107=LINE('',#28589,#2706);
#1108=LINE('',#28594,#2707);
#1109=LINE('',#28600,#2708);
#1110=LINE('',#28604,#2709);
#1111=LINE('',#28606,#2710);
#1112=LINE('',#28607,#2711);
#1113=LINE('',#28613,#2712);
#1114=LINE('',#28616,#2713);
#1115=LINE('',#28621,#2714);
#1116=LINE('',#28627,#2715);
#1117=LINE('',#28631,#2716);
#1118=LINE('',#28633,#2717);
#1119=LINE('',#28634,#2718);
#1120=LINE('',#28637,#2719);
#1121=LINE('',#28639,#2720);
#1122=LINE('',#28640,#2721);
#1123=LINE('',#28643,#2722);
#1124=LINE('',#28645,#2723);
#1125=LINE('',#28646,#2724);
#1126=LINE('',#28649,#2725);
#1127=LINE('',#28651,#2726);
#1128=LINE('',#28652,#2727);
#1129=LINE('',#28655,#2728);
#1130=LINE('',#28657,#2729);
#1131=LINE('',#28658,#2730);
#1132=LINE('',#28663,#2731);
#1133=LINE('',#28670,#2732);
#1134=LINE('',#28674,#2733);
#1135=LINE('',#28679,#2734);
#1136=LINE('',#28684,#2735);
#1137=LINE('',#28687,#2736);
#1138=LINE('',#28690,#2737);
#1139=LINE('',#28695,#2738);
#1140=LINE('',#28698,#2739);
#1141=LINE('',#28700,#2740);
#1142=LINE('',#28704,#2741);
#1143=LINE('',#28714,#2742);
#1144=LINE('',#28719,#2743);
#1145=LINE('',#28731,#2744);
#1146=LINE('',#28738,#2745);
#1147=LINE('',#28741,#2746);
#1148=LINE('',#28762,#2747);
#1149=LINE('',#28783,#2748);
#1150=LINE('',#28785,#2749);
#1151=LINE('',#28786,#2750);
#1152=LINE('',#28789,#2751);
#1153=LINE('',#28793,#2752);
#1154=LINE('',#28798,#2753);
#1155=LINE('',#28801,#2754);
#1156=LINE('',#28802,#2755);
#1157=LINE('',#28805,#2756);
#1158=LINE('',#28812,#2757);
#1159=LINE('',#28816,#2758);
#1160=LINE('',#28818,#2759);
#1161=LINE('',#28819,#2760);
#1162=LINE('',#28822,#2761);
#1163=LINE('',#28827,#2762);
#1164=LINE('',#28829,#2763);
#1165=LINE('',#28839,#2764);
#1166=LINE('',#28846,#2765);
#1167=LINE('',#28849,#2766);
#1168=LINE('',#28870,#2767);
#1169=LINE('',#28891,#2768);
#1170=LINE('',#28893,#2769);
#1171=LINE('',#28894,#2770);
#1172=LINE('',#28897,#2771);
#1173=LINE('',#28901,#2772);
#1174=LINE('',#28906,#2773);
#1175=LINE('',#28909,#2774);
#1176=LINE('',#28910,#2775);
#1177=LINE('',#28913,#2776);
#1178=LINE('',#28920,#2777);
#1179=LINE('',#28924,#2778);
#1180=LINE('',#28926,#2779);
#1181=LINE('',#28927,#2780);
#1182=LINE('',#28930,#2781);
#1183=LINE('',#28935,#2782);
#1184=LINE('',#28937,#2783);
#1185=LINE('',#28947,#2784);
#1186=LINE('',#28954,#2785);
#1187=LINE('',#28957,#2786);
#1188=LINE('',#28978,#2787);
#1189=LINE('',#28999,#2788);
#1190=LINE('',#29001,#2789);
#1191=LINE('',#29002,#2790);
#1192=LINE('',#29005,#2791);
#1193=LINE('',#29009,#2792);
#1194=LINE('',#29014,#2793);
#1195=LINE('',#29017,#2794);
#1196=LINE('',#29018,#2795);
#1197=LINE('',#29021,#2796);
#1198=LINE('',#29028,#2797);
#1199=LINE('',#29032,#2798);
#1200=LINE('',#29034,#2799);
#1201=LINE('',#29035,#2800);
#1202=LINE('',#29038,#2801);
#1203=LINE('',#29043,#2802);
#1204=LINE('',#29045,#2803);
#1205=LINE('',#29055,#2804);
#1206=LINE('',#29062,#2805);
#1207=LINE('',#29065,#2806);
#1208=LINE('',#29086,#2807);
#1209=LINE('',#29107,#2808);
#1210=LINE('',#29109,#2809);
#1211=LINE('',#29110,#2810);
#1212=LINE('',#29113,#2811);
#1213=LINE('',#29117,#2812);
#1214=LINE('',#29122,#2813);
#1215=LINE('',#29125,#2814);
#1216=LINE('',#29126,#2815);
#1217=LINE('',#29129,#2816);
#1218=LINE('',#29136,#2817);
#1219=LINE('',#29140,#2818);
#1220=LINE('',#29142,#2819);
#1221=LINE('',#29143,#2820);
#1222=LINE('',#29146,#2821);
#1223=LINE('',#29151,#2822);
#1224=LINE('',#29153,#2823);
#1225=LINE('',#29163,#2824);
#1226=LINE('',#29170,#2825);
#1227=LINE('',#29173,#2826);
#1228=LINE('',#29194,#2827);
#1229=LINE('',#29215,#2828);
#1230=LINE('',#29217,#2829);
#1231=LINE('',#29218,#2830);
#1232=LINE('',#29221,#2831);
#1233=LINE('',#29225,#2832);
#1234=LINE('',#29230,#2833);
#1235=LINE('',#29233,#2834);
#1236=LINE('',#29234,#2835);
#1237=LINE('',#29237,#2836);
#1238=LINE('',#29244,#2837);
#1239=LINE('',#29248,#2838);
#1240=LINE('',#29250,#2839);
#1241=LINE('',#29251,#2840);
#1242=LINE('',#29254,#2841);
#1243=LINE('',#29259,#2842);
#1244=LINE('',#29261,#2843);
#1245=LINE('',#29271,#2844);
#1246=LINE('',#29278,#2845);
#1247=LINE('',#29281,#2846);
#1248=LINE('',#29302,#2847);
#1249=LINE('',#29323,#2848);
#1250=LINE('',#29325,#2849);
#1251=LINE('',#29326,#2850);
#1252=LINE('',#29329,#2851);
#1253=LINE('',#29333,#2852);
#1254=LINE('',#29338,#2853);
#1255=LINE('',#29341,#2854);
#1256=LINE('',#29342,#2855);
#1257=LINE('',#29345,#2856);
#1258=LINE('',#29352,#2857);
#1259=LINE('',#29356,#2858);
#1260=LINE('',#29358,#2859);
#1261=LINE('',#29359,#2860);
#1262=LINE('',#29362,#2861);
#1263=LINE('',#29367,#2862);
#1264=LINE('',#29369,#2863);
#1265=LINE('',#29379,#2864);
#1266=LINE('',#29386,#2865);
#1267=LINE('',#29389,#2866);
#1268=LINE('',#29410,#2867);
#1269=LINE('',#29431,#2868);
#1270=LINE('',#29433,#2869);
#1271=LINE('',#29434,#2870);
#1272=LINE('',#29437,#2871);
#1273=LINE('',#29441,#2872);
#1274=LINE('',#29446,#2873);
#1275=LINE('',#29449,#2874);
#1276=LINE('',#29450,#2875);
#1277=LINE('',#29453,#2876);
#1278=LINE('',#29460,#2877);
#1279=LINE('',#29464,#2878);
#1280=LINE('',#29466,#2879);
#1281=LINE('',#29467,#2880);
#1282=LINE('',#29470,#2881);
#1283=LINE('',#29475,#2882);
#1284=LINE('',#29477,#2883);
#1285=LINE('',#29487,#2884);
#1286=LINE('',#29494,#2885);
#1287=LINE('',#29497,#2886);
#1288=LINE('',#29518,#2887);
#1289=LINE('',#29539,#2888);
#1290=LINE('',#29541,#2889);
#1291=LINE('',#29542,#2890);
#1292=LINE('',#29545,#2891);
#1293=LINE('',#29549,#2892);
#1294=LINE('',#29554,#2893);
#1295=LINE('',#29557,#2894);
#1296=LINE('',#29558,#2895);
#1297=LINE('',#29561,#2896);
#1298=LINE('',#29568,#2897);
#1299=LINE('',#29572,#2898);
#1300=LINE('',#29574,#2899);
#1301=LINE('',#29575,#2900);
#1302=LINE('',#29578,#2901);
#1303=LINE('',#29587,#2902);
#1304=LINE('',#29589,#2903);
#1305=LINE('',#29593,#2904);
#1306=LINE('',#29595,#2905);
#1307=LINE('',#29597,#2906);
#1308=LINE('',#29599,#2907);
#1309=LINE('',#29601,#2908);
#1310=LINE('',#29603,#2909);
#1311=LINE('',#29605,#2910);
#1312=LINE('',#29606,#2911);
#1313=LINE('',#29609,#2912);
#1314=LINE('',#29611,#2913);
#1315=LINE('',#29613,#2914);
#1316=LINE('',#29615,#2915);
#1317=LINE('',#29617,#2916);
#1318=LINE('',#29619,#2917);
#1319=LINE('',#29621,#2918);
#1320=LINE('',#29622,#2919);
#1321=LINE('',#29625,#2920);
#1322=LINE('',#29627,#2921);
#1323=LINE('',#29628,#2922);
#1324=LINE('',#29631,#2923);
#1325=LINE('',#29632,#2924);
#1326=LINE('',#29636,#2925);
#1327=LINE('',#29637,#2926);
#1328=LINE('',#29638,#2927);
#1329=LINE('',#29641,#2928);
#1330=LINE('',#29643,#2929);
#1331=LINE('',#29645,#2930);
#1332=LINE('',#29646,#2931);
#1333=LINE('',#29649,#2932);
#1334=LINE('',#29650,#2933);
#1335=LINE('',#29653,#2934);
#1336=LINE('',#29654,#2935);
#1337=LINE('',#29656,#2936);
#1338=LINE('',#29659,#2937);
#1339=LINE('',#29661,#2938);
#1340=LINE('',#29662,#2939);
#1341=LINE('',#29665,#2940);
#1342=LINE('',#29667,#2941);
#1343=LINE('',#29669,#2942);
#1344=LINE('',#29671,#2943);
#1345=LINE('',#29673,#2944);
#1346=LINE('',#29675,#2945);
#1347=LINE('',#29677,#2946);
#1348=LINE('',#29679,#2947);
#1349=LINE('',#29681,#2948);
#1350=LINE('',#29683,#2949);
#1351=LINE('',#29685,#2950);
#1352=LINE('',#29686,#2951);
#1353=LINE('',#29688,#2952);
#1354=LINE('',#29689,#2953);
#1355=LINE('',#29691,#2954);
#1356=LINE('',#29693,#2955);
#1357=LINE('',#29695,#2956);
#1358=LINE('',#29697,#2957);
#1359=LINE('',#29699,#2958);
#1360=LINE('',#29701,#2959);
#1361=LINE('',#29704,#2960);
#1362=LINE('',#29706,#2961);
#1363=LINE('',#29708,#2962);
#1364=LINE('',#29710,#2963);
#1365=LINE('',#29711,#2964);
#1366=LINE('',#29712,#2965);
#1367=LINE('',#29716,#2966);
#1368=LINE('',#29718,#2967);
#1369=LINE('',#29719,#2968);
#1370=LINE('',#29720,#2969);
#1371=LINE('',#29721,#2970);
#1372=LINE('',#29724,#2971);
#1373=LINE('',#29726,#2972);
#1374=LINE('',#29728,#2973);
#1375=LINE('',#29729,#2974);
#1376=LINE('',#29730,#2975);
#1377=LINE('',#29734,#2976);
#1378=LINE('',#29735,#2977);
#1379=LINE('',#29737,#2978);
#1380=LINE('',#29738,#2979);
#1381=LINE('',#29739,#2980);
#1382=LINE('',#29741,#2981);
#1383=LINE('',#29742,#2982);
#1384=LINE('',#29744,#2983);
#1385=LINE('',#29745,#2984);
#1386=LINE('',#29751,#2985);
#1387=LINE('',#29757,#2986);
#1388=LINE('',#29761,#2987);
#1389=LINE('',#29766,#2988);
#1390=LINE('',#29770,#2989);
#1391=LINE('',#29775,#2990);
#1392=LINE('',#29779,#2991);
#1393=LINE('',#29784,#2992);
#1394=LINE('',#29788,#2993);
#1395=LINE('',#29793,#2994);
#1396=LINE('',#29797,#2995);
#1397=LINE('',#29802,#2996);
#1398=LINE('',#29806,#2997);
#1399=LINE('',#29811,#2998);
#1400=LINE('',#29815,#2999);
#1401=LINE('',#29820,#3000);
#1402=LINE('',#29824,#3001);
#1403=LINE('',#29829,#3002);
#1404=LINE('',#29833,#3003);
#1405=LINE('',#29838,#3004);
#1406=LINE('',#29842,#3005);
#1407=LINE('',#29847,#3006);
#1408=LINE('',#29851,#3007);
#1409=LINE('',#29856,#3008);
#1410=LINE('',#29860,#3009);
#1411=LINE('',#29865,#3010);
#1412=LINE('',#29869,#3011);
#1413=LINE('',#29874,#3012);
#1414=LINE('',#29878,#3013);
#1415=LINE('',#29883,#3014);
#1416=LINE('',#29887,#3015);
#1417=LINE('',#29892,#3016);
#1418=LINE('',#29896,#3017);
#1419=LINE('',#29901,#3018);
#1420=LINE('',#29905,#3019);
#1421=LINE('',#29910,#3020);
#1422=LINE('',#29914,#3021);
#1423=LINE('',#29919,#3022);
#1424=LINE('',#29923,#3023);
#1425=LINE('',#29928,#3024);
#1426=LINE('',#29932,#3025);
#1427=LINE('',#29937,#3026);
#1428=LINE('',#29941,#3027);
#1429=LINE('',#29946,#3028);
#1430=LINE('',#29950,#3029);
#1431=LINE('',#29955,#3030);
#1432=LINE('',#29959,#3031);
#1433=LINE('',#29964,#3032);
#1434=LINE('',#29968,#3033);
#1435=LINE('',#29973,#3034);
#1436=LINE('',#29977,#3035);
#1437=LINE('',#29982,#3036);
#1438=LINE('',#29986,#3037);
#1439=LINE('',#29991,#3038);
#1440=LINE('',#29995,#3039);
#1441=LINE('',#30000,#3040);
#1442=LINE('',#30004,#3041);
#1443=LINE('',#30009,#3042);
#1444=LINE('',#30013,#3043);
#1445=LINE('',#30018,#3044);
#1446=LINE('',#30022,#3045);
#1447=LINE('',#30027,#3046);
#1448=LINE('',#30031,#3047);
#1449=LINE('',#30036,#3048);
#1450=LINE('',#30040,#3049);
#1451=LINE('',#30045,#3050);
#1452=LINE('',#30049,#3051);
#1453=LINE('',#30054,#3052);
#1454=LINE('',#30058,#3053);
#1455=LINE('',#30063,#3054);
#1456=LINE('',#30067,#3055);
#1457=LINE('',#30072,#3056);
#1458=LINE('',#30076,#3057);
#1459=LINE('',#30081,#3058);
#1460=LINE('',#30085,#3059);
#1461=LINE('',#30090,#3060);
#1462=LINE('',#30094,#3061);
#1463=LINE('',#30099,#3062);
#1464=LINE('',#30103,#3063);
#1465=LINE('',#30108,#3064);
#1466=LINE('',#30112,#3065);
#1467=LINE('',#30117,#3066);
#1468=LINE('',#30121,#3067);
#1469=LINE('',#30126,#3068);
#1470=LINE('',#30130,#3069);
#1471=LINE('',#30135,#3070);
#1472=LINE('',#30139,#3071);
#1473=LINE('',#30144,#3072);
#1474=LINE('',#30148,#3073);
#1475=LINE('',#30204,#3074);
#1476=LINE('',#30207,#3075);
#1477=LINE('',#30301,#3076);
#1478=LINE('',#30306,#3077);
#1479=LINE('',#30308,#3078);
#1480=LINE('',#30310,#3079);
#1481=LINE('',#30311,#3080);
#1482=LINE('',#30318,#3081);
#1483=LINE('',#30326,#3082);
#1484=LINE('',#30345,#3083);
#1485=LINE('',#30349,#3084);
#1486=LINE('',#30351,#3085);
#1487=LINE('',#30352,#3086);
#1488=LINE('',#30359,#3087);
#1489=LINE('',#30367,#3088);
#1490=LINE('',#30386,#3089);
#1491=LINE('',#30390,#3090);
#1492=LINE('',#30392,#3091);
#1493=LINE('',#30393,#3092);
#1494=LINE('',#30400,#3093);
#1495=LINE('',#30408,#3094);
#1496=LINE('',#30424,#3095);
#1497=LINE('',#30426,#3096);
#1498=LINE('',#30428,#3097);
#1499=LINE('',#30429,#3098);
#1500=LINE('',#30433,#3099);
#1501=LINE('',#30435,#3100);
#1502=LINE('',#30437,#3101);
#1503=LINE('',#30438,#3102);
#1504=LINE('',#30441,#3103);
#1505=LINE('',#30443,#3104);
#1506=LINE('',#30445,#3105);
#1507=LINE('',#30446,#3106);
#1508=LINE('',#30450,#3107);
#1509=LINE('',#30452,#3108);
#1510=LINE('',#30454,#3109);
#1511=LINE('',#30455,#3110);
#1512=LINE('',#30463,#3111);
#1513=LINE('',#30482,#3112);
#1514=LINE('',#30492,#3113);
#1515=LINE('',#30498,#3114);
#1516=LINE('',#30500,#3115);
#1517=LINE('',#30501,#3116);
#1518=LINE('',#30504,#3117);
#1519=LINE('',#30506,#3118);
#1520=LINE('',#30508,#3119);
#1521=LINE('',#30509,#3120);
#1522=LINE('',#30511,#3121);
#1523=LINE('',#30517,#3122);
#1524=LINE('',#30522,#3123);
#1525=LINE('',#30524,#3124);
#1526=LINE('',#30530,#3125);
#1527=LINE('',#30535,#3126);
#1528=LINE('',#30537,#3127);
#1529=LINE('',#30543,#3128);
#1530=LINE('',#30549,#3129);
#1531=LINE('',#30551,#3130);
#1532=LINE('',#30552,#3131);
#1533=LINE('',#30555,#3132);
#1534=LINE('',#30557,#3133);
#1535=LINE('',#30558,#3134);
#1536=LINE('',#30561,#3135);
#1537=LINE('',#30562,#3136);
#1538=LINE('',#30563,#3137);
#1539=LINE('',#30566,#3138);
#1540=LINE('',#30568,#3139);
#1541=LINE('',#30569,#3140);
#1542=LINE('',#30571,#3141);
#1543=LINE('',#30573,#3142);
#1544=LINE('',#30575,#3143);
#1545=LINE('',#30576,#3144);
#1546=LINE('',#30585,#3145);
#1547=LINE('',#30589,#3146);
#1548=LINE('',#30594,#3147);
#1549=LINE('',#30599,#3148);
#1550=LINE('',#30603,#3149);
#1551=LINE('',#30609,#3150);
#1552=LINE('',#30612,#3151);
#1553=LINE('',#30615,#3152);
#1554=LINE('',#30616,#3153);
#1555=LINE('',#30617,#3154);
#1556=LINE('',#30620,#3155);
#1557=LINE('',#30622,#3156);
#1558=LINE('',#30624,#3157);
#1559=LINE('',#30626,#3158);
#1560=LINE('',#30628,#3159);
#1561=LINE('',#30630,#3160);
#1562=LINE('',#30632,#3161);
#1563=LINE('',#30635,#3162);
#1564=LINE('',#30646,#3163);
#1565=LINE('',#30649,#3164);
#1566=LINE('',#30652,#3165);
#1567=LINE('',#30654,#3166);
#1568=LINE('',#30656,#3167);
#1569=LINE('',#30658,#3168);
#1570=LINE('',#30660,#3169);
#1571=LINE('',#30661,#3170);
#1572=LINE('',#30663,#3171);
#1573=LINE('',#30664,#3172);
#1574=LINE('',#30666,#3173);
#1575=LINE('',#30667,#3174);
#1576=LINE('',#30670,#3175);
#1577=LINE('',#30671,#3176);
#1578=LINE('',#30674,#3177);
#1579=LINE('',#30675,#3178);
#1580=LINE('',#30677,#3179);
#1581=LINE('',#30680,#3180);
#1582=LINE('',#30682,#3181);
#1583=LINE('',#30683,#3182);
#1584=LINE('',#30689,#3183);
#1585=LINE('',#30692,#3184);
#1586=LINE('',#30695,#3185);
#1587=LINE('',#30697,#3186);
#1588=LINE('',#30698,#3187);
#1589=LINE('',#30703,#3188);
#1590=LINE('',#30707,#3189);
#1591=LINE('',#30709,#3190);
#1592=LINE('',#30710,#3191);
#1593=LINE('',#30715,#3192);
#1594=LINE('',#30719,#3193);
#1595=LINE('',#30721,#3194);
#1596=LINE('',#30722,#3195);
#1597=LINE('',#30727,#3196);
#1598=LINE('',#30730,#3197);
#1599=LINE('',#30732,#3198);
#1600=LINE('',#30735,#3199);
#1601=LINE('',#30739,#3200);
#1602=LINE('',#30741,#3201);
#1603=LINE('',#30742,#3202);
#1604=LINE('',#30744,#3203);
#1605=LINE('',#30750,#3204);
#1606=LINE('',#30753,#3205);
#1607=LINE('',#30755,#3206);
#1608=LINE('',#30765,#3207);
#1609=LINE('',#30768,#3208);
#1610=LINE('',#30770,#3209);
#1611=LINE('',#30772,#3210);
#1612=LINE('',#30774,#3211);
#1613=LINE('',#30775,#3212);
#1614=LINE('',#30778,#3213);
#1615=LINE('',#30779,#3214);
#1616=LINE('',#30781,#3215);
#1617=LINE('',#30782,#3216);
#1618=LINE('',#30788,#3217);
#1619=LINE('',#30791,#3218);
#1620=LINE('',#30793,#3219);
#1621=LINE('',#30796,#3220);
#1622=LINE('',#30797,#3221);
#1623=LINE('',#30799,#3222);
#1624=LINE('',#30800,#3223);
#1625=LINE('',#30806,#3224);
#1626=LINE('',#30814,#3225);
#1627=LINE('',#30819,#3226);
#1628=LINE('',#30823,#3227);
#1629=LINE('',#30829,#3228);
#1630=LINE('',#30834,#3229);
#1631=LINE('',#30839,#3230);
#1632=LINE('',#30844,#3231);
#1633=LINE('',#30846,#3232);
#1634=LINE('',#30847,#3233);
#1635=LINE('',#30848,#3234);
#1636=LINE('',#30853,#3235);
#1637=LINE('',#30872,#3236);
#1638=LINE('',#30887,#3237);
#1639=LINE('',#30892,#3238);
#1640=LINE('',#30894,#3239);
#1641=LINE('',#30896,#3240);
#1642=LINE('',#30897,#3241);
#1643=LINE('',#30900,#3242);
#1644=LINE('',#30902,#3243);
#1645=LINE('',#30903,#3244);
#1646=LINE('',#30907,#3245);
#1647=LINE('',#30911,#3246);
#1648=LINE('',#30914,#3247);
#1649=LINE('',#30915,#3248);
#1650=LINE('',#30918,#3249);
#1651=LINE('',#30920,#3250);
#1652=LINE('',#30921,#3251);
#1653=LINE('',#30924,#3252);
#1654=LINE('',#30925,#3253);
#1655=LINE('',#30928,#3254);
#1656=LINE('',#30929,#3255);
#1657=LINE('',#30931,#3256);
#1658=LINE('',#30937,#3257);
#1659=LINE('',#30939,#3258);
#1660=LINE('',#30941,#3259);
#1661=LINE('',#30942,#3260);
#1662=LINE('',#30947,#3261);
#1663=LINE('',#30949,#3262);
#1664=LINE('',#30951,#3263);
#1665=LINE('',#30953,#3264);
#1666=LINE('',#30954,#3265);
#1667=LINE('',#30957,#3266);
#1668=LINE('',#30962,#3267);
#1669=LINE('',#30963,#3268);
#1670=LINE('',#30965,#3269);
#1671=LINE('',#30967,#3270);
#1672=LINE('',#30968,#3271);
#1673=LINE('',#30970,#3272);
#1674=LINE('',#30972,#3273);
#1675=LINE('',#30974,#3274);
#1676=LINE('',#30976,#3275);
#1677=LINE('',#30984,#3276);
#1678=LINE('',#30987,#3277);
#1679=LINE('',#30992,#3278);
#1680=LINE('',#30996,#3279);
#1681=LINE('',#30998,#3280);
#1682=LINE('',#30999,#3281);
#1683=LINE('',#31004,#3282);
#1684=LINE('',#31010,#3283);
#1685=LINE('',#31014,#3284);
#1686=LINE('',#31016,#3285);
#1687=LINE('',#31017,#3286);
#1688=LINE('',#31022,#3287);
#1689=LINE('',#31028,#3288);
#1690=LINE('',#31034,#3289);
#1691=LINE('',#31038,#3290);
#1692=LINE('',#31040,#3291);
#1693=LINE('',#31041,#3292);
#1694=LINE('',#31046,#3293);
#1695=LINE('',#31050,#3294);
#1696=LINE('',#31052,#3295);
#1697=LINE('',#31053,#3296);
#1698=LINE('',#31058,#3297);
#1699=LINE('',#31064,#3298);
#1700=LINE('',#31070,#3299);
#1701=LINE('',#31074,#3300);
#1702=LINE('',#31076,#3301);
#1703=LINE('',#31077,#3302);
#1704=LINE('',#31082,#3303);
#1705=LINE('',#31088,#3304);
#1706=LINE('',#31092,#3305);
#1707=LINE('',#31094,#3306);
#1708=LINE('',#31095,#3307);
#1709=LINE('',#31107,#3308);
#1710=LINE('',#31110,#3309);
#1711=LINE('',#31115,#3310);
#1712=LINE('',#31121,#3311);
#1713=LINE('',#31125,#3312);
#1714=LINE('',#31127,#3313);
#1715=LINE('',#31128,#3314);
#1716=LINE('',#31134,#3315);
#1717=LINE('',#31137,#3316);
#1718=LINE('',#31142,#3317);
#1719=LINE('',#31148,#3318);
#1720=LINE('',#31152,#3319);
#1721=LINE('',#31154,#3320);
#1722=LINE('',#31155,#3321);
#1723=LINE('',#31161,#3322);
#1724=LINE('',#31164,#3323);
#1725=LINE('',#31169,#3324);
#1726=LINE('',#31175,#3325);
#1727=LINE('',#31179,#3326);
#1728=LINE('',#31181,#3327);
#1729=LINE('',#31182,#3328);
#1730=LINE('',#31188,#3329);
#1731=LINE('',#31191,#3330);
#1732=LINE('',#31196,#3331);
#1733=LINE('',#31202,#3332);
#1734=LINE('',#31206,#3333);
#1735=LINE('',#31208,#3334);
#1736=LINE('',#31209,#3335);
#1737=LINE('',#31215,#3336);
#1738=LINE('',#31218,#3337);
#1739=LINE('',#31223,#3338);
#1740=LINE('',#31229,#3339);
#1741=LINE('',#31233,#3340);
#1742=LINE('',#31235,#3341);
#1743=LINE('',#31236,#3342);
#1744=LINE('',#31239,#3343);
#1745=LINE('',#31241,#3344);
#1746=LINE('',#31242,#3345);
#1747=LINE('',#31245,#3346);
#1748=LINE('',#31247,#3347);
#1749=LINE('',#31248,#3348);
#1750=LINE('',#31251,#3349);
#1751=LINE('',#31253,#3350);
#1752=LINE('',#31254,#3351);
#1753=LINE('',#31257,#3352);
#1754=LINE('',#31259,#3353);
#1755=LINE('',#31260,#3354);
#1756=LINE('',#31265,#3355);
#1757=LINE('',#31272,#3356);
#1758=LINE('',#31276,#3357);
#1759=LINE('',#31281,#3358);
#1760=LINE('',#31286,#3359);
#1761=LINE('',#31289,#3360);
#1762=LINE('',#31292,#3361);
#1763=LINE('',#31297,#3362);
#1764=LINE('',#31298,#3363);
#1765=LINE('',#31302,#3364);
#1766=LINE('',#31304,#3365);
#1767=LINE('',#31314,#3366);
#1768=LINE('',#31322,#3367);
#1769=LINE('',#31333,#3368);
#1770=LINE('',#31341,#3369);
#1771=LINE('',#31352,#3370);
#1772=LINE('',#31360,#3371);
#1773=LINE('',#31371,#3372);
#1774=LINE('',#31379,#3373);
#1775=LINE('',#31410,#3374);
#1776=LINE('',#31411,#3375);
#1777=LINE('',#31413,#3376);
#1778=LINE('',#31415,#3377);
#1779=LINE('',#31416,#3378);
#1780=LINE('',#31418,#3379);
#1781=LINE('',#31420,#3380);
#1782=LINE('',#31421,#3381);
#1783=LINE('',#31423,#3382);
#1784=LINE('',#31426,#3383);
#1785=LINE('',#31428,#3384);
#1786=LINE('',#31430,#3385);
#1787=LINE('',#31432,#3386);
#1788=LINE('',#31434,#3387);
#1789=LINE('',#31436,#3388);
#1790=LINE('',#31438,#3389);
#1791=LINE('',#31439,#3390);
#1792=LINE('',#31449,#3391);
#1793=LINE('',#31451,#3392);
#1794=LINE('',#31465,#3393);
#1795=LINE('',#31467,#3394);
#1796=LINE('',#31469,#3395);
#1797=LINE('',#31470,#3396);
#1798=LINE('',#31473,#3397);
#1799=LINE('',#31475,#3398);
#1800=LINE('',#31476,#3399);
#1801=LINE('',#31479,#3400);
#1802=LINE('',#31481,#3401);
#1803=LINE('',#31482,#3402);
#1804=LINE('',#31485,#3403);
#1805=LINE('',#31487,#3404);
#1806=LINE('',#31488,#3405);
#1807=LINE('',#31491,#3406);
#1808=LINE('',#31493,#3407);
#1809=LINE('',#31494,#3408);
#1810=LINE('',#31497,#3409);
#1811=LINE('',#31499,#3410);
#1812=LINE('',#31500,#3411);
#1813=LINE('',#31503,#3412);
#1814=LINE('',#31505,#3413);
#1815=LINE('',#31506,#3414);
#1816=LINE('',#31508,#3415);
#1817=LINE('',#31509,#3416);
#1818=LINE('',#31511,#3417);
#1819=LINE('',#31512,#3418);
#1820=LINE('',#31514,#3419);
#1821=LINE('',#31516,#3420);
#1822=LINE('',#31518,#3421);
#1823=LINE('',#31523,#3422);
#1824=LINE('',#31529,#3423);
#1825=LINE('',#31536,#3424);
#1826=LINE('',#31541,#3425);
#1827=LINE('',#31546,#3426);
#1828=LINE('',#31549,#3427);
#1829=LINE('',#31558,#3428);
#1830=LINE('',#31564,#3429);
#1831=LINE('',#31569,#3430);
#1832=LINE('',#31573,#3431);
#1833=LINE('',#31576,#3432);
#1834=LINE('',#31578,#3433);
#1835=LINE('',#31580,#3434);
#1836=LINE('',#31582,#3435);
#1837=LINE('',#31586,#3436);
#1838=LINE('',#31589,#3437);
#1839=LINE('',#31591,#3438);
#1840=LINE('',#31593,#3439);
#1841=LINE('',#31602,#3440);
#1842=LINE('',#31605,#3441);
#1843=LINE('',#31610,#3442);
#1844=LINE('',#31616,#3443);
#1845=LINE('',#31620,#3444);
#1846=LINE('',#31622,#3445);
#1847=LINE('',#31623,#3446);
#1848=LINE('',#31629,#3447);
#1849=LINE('',#31632,#3448);
#1850=LINE('',#31637,#3449);
#1851=LINE('',#31643,#3450);
#1852=LINE('',#31647,#3451);
#1853=LINE('',#31649,#3452);
#1854=LINE('',#31650,#3453);
#1855=LINE('',#31656,#3454);
#1856=LINE('',#31659,#3455);
#1857=LINE('',#31664,#3456);
#1858=LINE('',#31670,#3457);
#1859=LINE('',#31674,#3458);
#1860=LINE('',#31676,#3459);
#1861=LINE('',#31677,#3460);
#1862=LINE('',#31683,#3461);
#1863=LINE('',#31686,#3462);
#1864=LINE('',#31691,#3463);
#1865=LINE('',#31697,#3464);
#1866=LINE('',#31701,#3465);
#1867=LINE('',#31703,#3466);
#1868=LINE('',#31704,#3467);
#1869=LINE('',#31710,#3468);
#1870=LINE('',#31713,#3469);
#1871=LINE('',#31718,#3470);
#1872=LINE('',#31724,#3471);
#1873=LINE('',#31728,#3472);
#1874=LINE('',#31730,#3473);
#1875=LINE('',#31731,#3474);
#1876=LINE('',#31734,#3475);
#1877=LINE('',#31736,#3476);
#1878=LINE('',#31737,#3477);
#1879=LINE('',#31740,#3478);
#1880=LINE('',#31742,#3479);
#1881=LINE('',#31743,#3480);
#1882=LINE('',#31746,#3481);
#1883=LINE('',#31748,#3482);
#1884=LINE('',#31749,#3483);
#1885=LINE('',#31752,#3484);
#1886=LINE('',#31754,#3485);
#1887=LINE('',#31755,#3486);
#1888=LINE('',#31760,#3487);
#1889=LINE('',#31767,#3488);
#1890=LINE('',#31771,#3489);
#1891=LINE('',#31776,#3490);
#1892=LINE('',#31781,#3491);
#1893=LINE('',#31784,#3492);
#1894=LINE('',#31787,#3493);
#1895=LINE('',#31792,#3494);
#1896=LINE('',#31793,#3495);
#1897=LINE('',#31797,#3496);
#1898=LINE('',#31799,#3497);
#1899=LINE('',#31807,#3498);
#1900=LINE('',#31828,#3499);
#1901=LINE('',#31838,#3500);
#1902=LINE('',#31839,#3501);
#1903=LINE('',#31841,#3502);
#1904=LINE('',#31844,#3503);
#1905=LINE('',#31848,#3504);
#1906=LINE('',#31854,#3505);
#1907=LINE('',#31862,#3506);
#1908=LINE('',#31864,#3507);
#1909=LINE('',#31866,#3508);
#1910=LINE('',#31867,#3509);
#1911=LINE('',#31871,#3510);
#1912=LINE('',#31873,#3511);
#1913=LINE('',#31875,#3512);
#1914=LINE('',#31876,#3513);
#1915=LINE('',#31879,#3514);
#1916=LINE('',#31881,#3515);
#1917=LINE('',#31882,#3516);
#1918=LINE('',#31885,#3517);
#1919=LINE('',#31887,#3518);
#1920=LINE('',#31888,#3519);
#1921=LINE('',#31891,#3520);
#1922=LINE('',#31893,#3521);
#1923=LINE('',#31894,#3522);
#1924=LINE('',#31896,#3523);
#1925=LINE('',#31898,#3524);
#1926=LINE('',#31900,#3525);
#1927=LINE('',#31902,#3526);
#1928=LINE('',#31904,#3527);
#1929=LINE('',#31908,#3528);
#1930=LINE('',#31910,#3529);
#1931=LINE('',#31911,#3530);
#1932=LINE('',#31914,#3531);
#1933=LINE('',#31915,#3532);
#1934=LINE('',#31918,#3533);
#1935=LINE('',#31920,#3534);
#1936=LINE('',#31921,#3535);
#1937=LINE('',#31924,#3536);
#1938=LINE('',#31925,#3537);
#1939=LINE('',#31927,#3538);
#1940=LINE('',#31929,#3539);
#1941=LINE('',#31933,#3540);
#1942=LINE('',#31936,#3541);
#1943=LINE('',#31937,#3542);
#1944=LINE('',#31940,#3543);
#1945=LINE('',#31941,#3544);
#1946=LINE('',#31943,#3545);
#1947=LINE('',#31950,#3546);
#1948=LINE('',#31956,#3547);
#1949=LINE('',#31962,#3548);
#1950=LINE('',#31968,#3549);
#1951=LINE('',#31974,#3550);
#1952=LINE('',#31980,#3551);
#1953=LINE('',#31986,#3552);
#1954=LINE('',#31992,#3553);
#1955=LINE('',#31998,#3554);
#1956=LINE('',#32004,#3555);
#1957=LINE('',#32009,#3556);
#1958=LINE('',#32011,#3557);
#1959=LINE('',#32013,#3558);
#1960=LINE('',#32014,#3559);
#1961=LINE('',#32017,#3560);
#1962=LINE('',#32019,#3561);
#1963=LINE('',#32020,#3562);
#1964=LINE('',#32024,#3563);
#1965=LINE('',#32026,#3564);
#1966=LINE('',#32028,#3565);
#1967=LINE('',#32029,#3566);
#1968=LINE('',#32031,#3567);
#1969=LINE('',#32032,#3568);
#1970=LINE('',#32036,#3569);
#1971=LINE('',#32038,#3570);
#1972=LINE('',#32040,#3571);
#1973=LINE('',#32041,#3572);
#1974=LINE('',#32044,#3573);
#1975=LINE('',#32046,#3574);
#1976=LINE('',#32047,#3575);
#1977=LINE('',#32049,#3576);
#1978=LINE('',#32050,#3577);
#1979=LINE('',#32056,#3578);
#1980=LINE('',#32059,#3579);
#1981=LINE('',#32061,#3580);
#1982=LINE('',#32062,#3581);
#1983=LINE('',#32064,#3582);
#1984=LINE('',#32065,#3583);
#1985=LINE('',#32072,#3584);
#1986=LINE('',#32074,#3585);
#1987=LINE('',#32076,#3586);
#1988=LINE('',#32077,#3587);
#1989=LINE('',#32080,#3588);
#1990=LINE('',#32082,#3589);
#1991=LINE('',#32083,#3590);
#1992=LINE('',#32087,#3591);
#1993=LINE('',#32091,#3592);
#1994=LINE('',#32094,#3593);
#1995=LINE('',#32095,#3594);
#1996=LINE('',#32098,#3595);
#1997=LINE('',#32100,#3596);
#1998=LINE('',#32101,#3597);
#1999=LINE('',#32104,#3598);
#2000=LINE('',#32105,#3599);
#2001=LINE('',#32108,#3600);
#2002=LINE('',#32109,#3601);
#2003=LINE('',#32111,#3602);
#2004=LINE('',#32119,#3603);
#2005=LINE('',#32122,#3604);
#2006=LINE('',#32127,#3605);
#2007=LINE('',#32133,#3606);
#2008=LINE('',#32137,#3607);
#2009=LINE('',#32139,#3608);
#2010=LINE('',#32140,#3609);
#2011=LINE('',#32146,#3610);
#2012=LINE('',#32149,#3611);
#2013=LINE('',#32154,#3612);
#2014=LINE('',#32160,#3613);
#2015=LINE('',#32164,#3614);
#2016=LINE('',#32166,#3615);
#2017=LINE('',#32167,#3616);
#2018=LINE('',#32173,#3617);
#2019=LINE('',#32176,#3618);
#2020=LINE('',#32181,#3619);
#2021=LINE('',#32187,#3620);
#2022=LINE('',#32191,#3621);
#2023=LINE('',#32193,#3622);
#2024=LINE('',#32194,#3623);
#2025=LINE('',#32200,#3624);
#2026=LINE('',#32203,#3625);
#2027=LINE('',#32208,#3626);
#2028=LINE('',#32214,#3627);
#2029=LINE('',#32218,#3628);
#2030=LINE('',#32220,#3629);
#2031=LINE('',#32221,#3630);
#2032=LINE('',#32227,#3631);
#2033=LINE('',#32230,#3632);
#2034=LINE('',#32235,#3633);
#2035=LINE('',#32241,#3634);
#2036=LINE('',#32245,#3635);
#2037=LINE('',#32247,#3636);
#2038=LINE('',#32248,#3637);
#2039=LINE('',#32251,#3638);
#2040=LINE('',#32253,#3639);
#2041=LINE('',#32254,#3640);
#2042=LINE('',#32257,#3641);
#2043=LINE('',#32259,#3642);
#2044=LINE('',#32260,#3643);
#2045=LINE('',#32263,#3644);
#2046=LINE('',#32265,#3645);
#2047=LINE('',#32266,#3646);
#2048=LINE('',#32269,#3647);
#2049=LINE('',#32271,#3648);
#2050=LINE('',#32272,#3649);
#2051=LINE('',#32277,#3650);
#2052=LINE('',#32284,#3651);
#2053=LINE('',#32288,#3652);
#2054=LINE('',#32293,#3653);
#2055=LINE('',#32298,#3654);
#2056=LINE('',#32301,#3655);
#2057=LINE('',#32304,#3656);
#2058=LINE('',#32309,#3657);
#2059=LINE('',#32312,#3658);
#2060=LINE('',#32314,#3659);
#2061=LINE('',#32318,#3660);
#2062=LINE('',#32328,#3661);
#2063=LINE('',#32333,#3662);
#2064=LINE('',#32339,#3663);
#2065=LINE('',#32341,#3664);
#2066=LINE('',#32343,#3665);
#2067=LINE('',#32344,#3666);
#2068=LINE('',#32347,#3667);
#2069=LINE('',#32349,#3668);
#2070=LINE('',#32350,#3669);
#2071=LINE('',#32353,#3670);
#2072=LINE('',#32357,#3671);
#2073=LINE('',#32359,#3672);
#2074=LINE('',#32360,#3673);
#2075=LINE('',#32363,#3674);
#2076=LINE('',#32365,#3675);
#2077=LINE('',#32368,#3676);
#2078=LINE('',#32370,#3677);
#2079=LINE('',#32372,#3678);
#2080=LINE('',#32373,#3679);
#2081=LINE('',#32376,#3680);
#2082=LINE('',#32378,#3681);
#2083=LINE('',#32384,#3682);
#2084=LINE('',#32388,#3683);
#2085=LINE('',#32393,#3684);
#2086=LINE('',#32397,#3685);
#2087=LINE('',#32402,#3686);
#2088=LINE('',#32406,#3687);
#2089=LINE('',#32411,#3688);
#2090=LINE('',#32415,#3689);
#2091=LINE('',#32420,#3690);
#2092=LINE('',#32424,#3691);
#2093=LINE('',#32429,#3692);
#2094=LINE('',#32433,#3693);
#2095=LINE('',#32438,#3694);
#2096=LINE('',#32442,#3695);
#2097=LINE('',#32447,#3696);
#2098=LINE('',#32451,#3697);
#2099=LINE('',#32456,#3698);
#2100=LINE('',#32460,#3699);
#2101=LINE('',#32465,#3700);
#2102=LINE('',#32469,#3701);
#2103=LINE('',#32474,#3702);
#2104=LINE('',#32478,#3703);
#2105=LINE('',#32483,#3704);
#2106=LINE('',#32487,#3705);
#2107=LINE('',#32492,#3706);
#2108=LINE('',#32496,#3707);
#2109=LINE('',#32501,#3708);
#2110=LINE('',#32505,#3709);
#2111=LINE('',#32510,#3710);
#2112=LINE('',#32514,#3711);
#2113=LINE('',#32519,#3712);
#2114=LINE('',#32523,#3713);
#2115=LINE('',#32528,#3714);
#2116=LINE('',#32532,#3715);
#2117=LINE('',#32537,#3716);
#2118=LINE('',#32541,#3717);
#2119=LINE('',#32546,#3718);
#2120=LINE('',#32550,#3719);
#2121=LINE('',#32555,#3720);
#2122=LINE('',#32559,#3721);
#2123=LINE('',#32564,#3722);
#2124=LINE('',#32568,#3723);
#2125=LINE('',#32573,#3724);
#2126=LINE('',#32577,#3725);
#2127=LINE('',#32582,#3726);
#2128=LINE('',#32586,#3727);
#2129=LINE('',#32591,#3728);
#2130=LINE('',#32595,#3729);
#2131=LINE('',#32600,#3730);
#2132=LINE('',#32604,#3731);
#2133=LINE('',#32609,#3732);
#2134=LINE('',#32613,#3733);
#2135=LINE('',#32618,#3734);
#2136=LINE('',#32622,#3735);
#2137=LINE('',#32627,#3736);
#2138=LINE('',#32631,#3737);
#2139=LINE('',#32636,#3738);
#2140=LINE('',#32640,#3739);
#2141=LINE('',#32645,#3740);
#2142=LINE('',#32649,#3741);
#2143=LINE('',#32654,#3742);
#2144=LINE('',#32658,#3743);
#2145=LINE('',#32663,#3744);
#2146=LINE('',#32667,#3745);
#2147=LINE('',#32672,#3746);
#2148=LINE('',#32676,#3747);
#2149=LINE('',#32681,#3748);
#2150=LINE('',#32685,#3749);
#2151=LINE('',#32690,#3750);
#2152=LINE('',#32694,#3751);
#2153=LINE('',#32699,#3752);
#2154=LINE('',#32703,#3753);
#2155=LINE('',#32708,#3754);
#2156=LINE('',#32712,#3755);
#2157=LINE('',#32717,#3756);
#2158=LINE('',#32721,#3757);
#2159=LINE('',#32726,#3758);
#2160=LINE('',#32730,#3759);
#2161=LINE('',#32735,#3760);
#2162=LINE('',#32739,#3761);
#2163=LINE('',#32744,#3762);
#2164=LINE('',#32748,#3763);
#2165=LINE('',#32753,#3764);
#2166=LINE('',#32757,#3765);
#2167=LINE('',#32762,#3766);
#2168=LINE('',#32766,#3767);
#2169=LINE('',#32771,#3768);
#2170=LINE('',#32775,#3769);
#2171=LINE('',#32831,#3770);
#2172=LINE('',#32834,#3771);
#2173=LINE('',#32928,#3772);
#2174=LINE('',#32942,#3773);
#2175=LINE('',#32955,#3774);
#2176=LINE('',#32962,#3775);
#2177=LINE('',#32965,#3776);
#2178=LINE('',#32970,#3777);
#2179=LINE('',#32976,#3778);
#2180=LINE('',#32980,#3779);
#2181=LINE('',#32982,#3780);
#2182=LINE('',#32983,#3781);
#2183=LINE('',#32989,#3782);
#2184=LINE('',#32992,#3783);
#2185=LINE('',#32997,#3784);
#2186=LINE('',#33003,#3785);
#2187=LINE('',#33007,#3786);
#2188=LINE('',#33009,#3787);
#2189=LINE('',#33010,#3788);
#2190=LINE('',#33016,#3789);
#2191=LINE('',#33019,#3790);
#2192=LINE('',#33024,#3791);
#2193=LINE('',#33030,#3792);
#2194=LINE('',#33034,#3793);
#2195=LINE('',#33036,#3794);
#2196=LINE('',#33037,#3795);
#2197=LINE('',#33043,#3796);
#2198=LINE('',#33046,#3797);
#2199=LINE('',#33051,#3798);
#2200=LINE('',#33057,#3799);
#2201=LINE('',#33061,#3800);
#2202=LINE('',#33063,#3801);
#2203=LINE('',#33064,#3802);
#2204=LINE('',#33070,#3803);
#2205=LINE('',#33073,#3804);
#2206=LINE('',#33078,#3805);
#2207=LINE('',#33084,#3806);
#2208=LINE('',#33088,#3807);
#2209=LINE('',#33090,#3808);
#2210=LINE('',#33091,#3809);
#2211=LINE('',#33094,#3810);
#2212=LINE('',#33096,#3811);
#2213=LINE('',#33097,#3812);
#2214=LINE('',#33100,#3813);
#2215=LINE('',#33102,#3814);
#2216=LINE('',#33103,#3815);
#2217=LINE('',#33106,#3816);
#2218=LINE('',#33108,#3817);
#2219=LINE('',#33109,#3818);
#2220=LINE('',#33112,#3819);
#2221=LINE('',#33114,#3820);
#2222=LINE('',#33115,#3821);
#2223=LINE('',#33120,#3822);
#2224=LINE('',#33127,#3823);
#2225=LINE('',#33131,#3824);
#2226=LINE('',#33136,#3825);
#2227=LINE('',#33141,#3826);
#2228=LINE('',#33144,#3827);
#2229=LINE('',#33147,#3828);
#2230=LINE('',#33152,#3829);
#2231=LINE('',#33153,#3830);
#2232=LINE('',#33157,#3831);
#2233=LINE('',#33159,#3832);
#2234=LINE('',#33167,#3833);
#2235=LINE('',#33169,#3834);
#2236=LINE('',#33171,#3835);
#2237=LINE('',#33172,#3836);
#2238=LINE('',#33176,#3837);
#2239=LINE('',#33178,#3838);
#2240=LINE('',#33180,#3839);
#2241=LINE('',#33181,#3840);
#2242=LINE('',#33183,#3841);
#2243=LINE('',#33184,#3842);
#2244=LINE('',#33189,#3843);
#2245=LINE('',#33191,#3844);
#2246=LINE('',#33192,#3845);
#2247=LINE('',#33195,#3846);
#2248=LINE('',#33199,#3847);
#2249=LINE('',#33201,#3848);
#2250=LINE('',#33202,#3849);
#2251=LINE('',#33204,#3850);
#2252=LINE('',#33206,#3851);
#2253=LINE('',#33212,#3852);
#2254=LINE('',#33216,#3853);
#2255=LINE('',#33221,#3854);
#2256=LINE('',#33222,#3855);
#2257=LINE('',#33223,#3856);
#2258=LINE('',#33227,#3857);
#2259=LINE('',#33233,#3858);
#2260=LINE('',#33239,#3859);
#2261=LINE('',#33245,#3860);
#2262=LINE('',#33246,#3861);
#2263=LINE('',#33247,#3862);
#2264=LINE('',#33251,#3863);
#2265=LINE('',#33257,#3864);
#2266=LINE('',#33263,#3865);
#2267=LINE('',#33267,#3866);
#2268=LINE('',#33271,#3867);
#2269=LINE('',#33273,#3868);
#2270=LINE('',#33274,#3869);
#2271=LINE('',#33279,#3870);
#2272=LINE('',#33285,#3871);
#2273=LINE('',#33291,#3872);
#2274=LINE('',#33295,#3873);
#2275=LINE('',#33297,#3874);
#2276=LINE('',#33298,#3875);
#2277=LINE('',#33314,#3876);
#2278=LINE('',#33316,#3877);
#2279=LINE('',#33318,#3878);
#2280=LINE('',#33320,#3879);
#2281=LINE('',#33322,#3880);
#2282=LINE('',#33324,#3881);
#2283=LINE('',#33326,#3882);
#2284=LINE('',#33327,#3883);
#2285=LINE('',#33332,#3884);
#2286=LINE('',#33336,#3885);
#2287=LINE('',#33340,#3886);
#2288=LINE('',#33344,#3887);
#2289=LINE('',#33348,#3888);
#2290=LINE('',#33350,#3889);
#2291=LINE('',#33351,#3890);
#2292=LINE('',#33354,#3891);
#2293=LINE('',#33355,#3892);
#2294=LINE('',#33358,#3893);
#2295=LINE('',#33359,#3894);
#2296=LINE('',#33362,#3895);
#2297=LINE('',#33363,#3896);
#2298=LINE('',#33366,#3897);
#2299=LINE('',#33367,#3898);
#2300=LINE('',#33370,#3899);
#2301=LINE('',#33371,#3900);
#2302=LINE('',#33374,#3901);
#2303=LINE('',#33375,#3902);
#2304=LINE('',#33377,#3903);
#2305=LINE('',#33385,#3904);
#2306=LINE('',#33388,#3905);
#2307=LINE('',#33393,#3906);
#2308=LINE('',#33399,#3907);
#2309=LINE('',#33403,#3908);
#2310=LINE('',#33405,#3909);
#2311=LINE('',#33406,#3910);
#2312=LINE('',#33412,#3911);
#2313=LINE('',#33415,#3912);
#2314=LINE('',#33420,#3913);
#2315=LINE('',#33426,#3914);
#2316=LINE('',#33430,#3915);
#2317=LINE('',#33432,#3916);
#2318=LINE('',#33433,#3917);
#2319=LINE('',#33439,#3918);
#2320=LINE('',#33442,#3919);
#2321=LINE('',#33447,#3920);
#2322=LINE('',#33453,#3921);
#2323=LINE('',#33457,#3922);
#2324=LINE('',#33459,#3923);
#2325=LINE('',#33460,#3924);
#2326=LINE('',#33466,#3925);
#2327=LINE('',#33469,#3926);
#2328=LINE('',#33474,#3927);
#2329=LINE('',#33480,#3928);
#2330=LINE('',#33484,#3929);
#2331=LINE('',#33486,#3930);
#2332=LINE('',#33487,#3931);
#2333=LINE('',#33493,#3932);
#2334=LINE('',#33496,#3933);
#2335=LINE('',#33501,#3934);
#2336=LINE('',#33507,#3935);
#2337=LINE('',#33511,#3936);
#2338=LINE('',#33513,#3937);
#2339=LINE('',#33514,#3938);
#2340=LINE('',#33517,#3939);
#2341=LINE('',#33519,#3940);
#2342=LINE('',#33520,#3941);
#2343=LINE('',#33523,#3942);
#2344=LINE('',#33525,#3943);
#2345=LINE('',#33526,#3944);
#2346=LINE('',#33529,#3945);
#2347=LINE('',#33531,#3946);
#2348=LINE('',#33532,#3947);
#2349=LINE('',#33535,#3948);
#2350=LINE('',#33537,#3949);
#2351=LINE('',#33538,#3950);
#2352=LINE('',#33543,#3951);
#2353=LINE('',#33550,#3952);
#2354=LINE('',#33554,#3953);
#2355=LINE('',#33559,#3954);
#2356=LINE('',#33564,#3955);
#2357=LINE('',#33567,#3956);
#2358=LINE('',#33570,#3957);
#2359=LINE('',#33575,#3958);
#2360=LINE('',#33578,#3959);
#2361=LINE('',#33580,#3960);
#2362=LINE('',#33584,#3961);
#2363=LINE('',#33590,#3962);
#2364=LINE('',#33592,#3963);
#2365=LINE('',#33594,#3964);
#2366=LINE('',#33595,#3965);
#2367=LINE('',#33598,#3966);
#2368=LINE('',#33600,#3967);
#2369=LINE('',#33601,#3968);
#2370=LINE('',#33604,#3969);
#2371=LINE('',#33606,#3970);
#2372=LINE('',#33607,#3971);
#2373=LINE('',#33609,#3972);
#2374=LINE('',#33610,#3973);
#2375=LINE('',#33614,#3974);
#2376=LINE('',#33616,#3975);
#2377=LINE('',#33618,#3976);
#2378=LINE('',#33619,#3977);
#2379=LINE('',#33622,#3978);
#2380=LINE('',#33624,#3979);
#2381=LINE('',#33625,#3980);
#2382=LINE('',#33628,#3981);
#2383=LINE('',#33630,#3982);
#2384=LINE('',#33631,#3983);
#2385=LINE('',#33633,#3984);
#2386=LINE('',#33634,#3985);
#2387=LINE('',#33638,#3986);
#2388=LINE('',#33640,#3987);
#2389=LINE('',#33642,#3988);
#2390=LINE('',#33643,#3989);
#2391=LINE('',#33646,#3990);
#2392=LINE('',#33648,#3991);
#2393=LINE('',#33649,#3992);
#2394=LINE('',#33652,#3993);
#2395=LINE('',#33654,#3994);
#2396=LINE('',#33655,#3995);
#2397=LINE('',#33657,#3996);
#2398=LINE('',#33658,#3997);
#2399=LINE('',#33662,#3998);
#2400=LINE('',#33664,#3999);
#2401=LINE('',#33666,#4000);
#2402=LINE('',#33667,#4001);
#2403=LINE('',#33670,#4002);
#2404=LINE('',#33672,#4003);
#2405=LINE('',#33673,#4004);
#2406=LINE('',#33676,#4005);
#2407=LINE('',#33678,#4006);
#2408=LINE('',#33679,#4007);
#2409=LINE('',#33681,#4008);
#2410=LINE('',#33682,#4009);
#2411=LINE('',#33686,#4010);
#2412=LINE('',#33688,#4011);
#2413=LINE('',#33690,#4012);
#2414=LINE('',#33691,#4013);
#2415=LINE('',#33694,#4014);
#2416=LINE('',#33696,#4015);
#2417=LINE('',#33697,#4016);
#2418=LINE('',#33700,#4017);
#2419=LINE('',#33702,#4018);
#2420=LINE('',#33703,#4019);
#2421=LINE('',#33705,#4020);
#2422=LINE('',#33706,#4021);
#2423=LINE('',#33710,#4022);
#2424=LINE('',#33712,#4023);
#2425=LINE('',#33714,#4024);
#2426=LINE('',#33715,#4025);
#2427=LINE('',#33718,#4026);
#2428=LINE('',#33720,#4027);
#2429=LINE('',#33721,#4028);
#2430=LINE('',#33724,#4029);
#2431=LINE('',#33726,#4030);
#2432=LINE('',#33727,#4031);
#2433=LINE('',#33729,#4032);
#2434=LINE('',#33730,#4033);
#2435=LINE('',#33734,#4034);
#2436=LINE('',#33736,#4035);
#2437=LINE('',#33738,#4036);
#2438=LINE('',#33739,#4037);
#2439=LINE('',#33742,#4038);
#2440=LINE('',#33744,#4039);
#2441=LINE('',#33745,#4040);
#2442=LINE('',#33748,#4041);
#2443=LINE('',#33750,#4042);
#2444=LINE('',#33751,#4043);
#2445=LINE('',#33754,#4044);
#2446=LINE('',#33756,#4045);
#2447=LINE('',#33758,#4046);
#2448=LINE('',#33760,#4047);
#2449=LINE('',#33761,#4048);
#2450=LINE('',#33764,#4049);
#2451=LINE('',#33766,#4050);
#2452=LINE('',#33768,#4051);
#2453=LINE('',#33769,#4052);
#2454=LINE('',#33772,#4053);
#2455=LINE('',#33774,#4054);
#2456=LINE('',#33775,#4055);
#2457=LINE('',#33778,#4056);
#2458=LINE('',#33780,#4057);
#2459=LINE('',#33782,#4058);
#2460=LINE('',#33784,#4059);
#2461=LINE('',#33786,#4060);
#2462=LINE('',#33788,#4061);
#2463=LINE('',#33790,#4062);
#2464=LINE('',#33792,#4063);
#2465=LINE('',#33794,#4064);
#2466=LINE('',#33795,#4065);
#2467=LINE('',#33799,#4066);
#2468=LINE('',#33800,#4067);
#2469=LINE('',#33801,#4068);
#2470=LINE('',#33805,#4069);
#2471=LINE('',#33807,#4070);
#2472=LINE('',#33809,#4071);
#2473=LINE('',#33810,#4072);
#2474=LINE('',#33812,#4073);
#2475=LINE('',#33813,#4074);
#2476=LINE('',#33816,#4075);
#2477=LINE('',#33818,#4076);
#2478=LINE('',#33820,#4077);
#2479=LINE('',#33821,#4078);
#2480=LINE('',#33823,#4079);
#2481=LINE('',#33825,#4080);
#2482=LINE('',#33827,#4081);
#2483=LINE('',#33828,#4082);
#2484=LINE('',#33830,#4083);
#2485=LINE('',#33832,#4084);
#2486=LINE('',#33834,#4085);
#2487=LINE('',#33836,#4086);
#2488=LINE('',#33837,#4087);
#2489=LINE('',#33841,#4088);
#2490=LINE('',#33842,#4089);
#2491=LINE('',#33843,#4090);
#2492=LINE('',#33846,#4091);
#2493=LINE('',#33848,#4092);
#2494=LINE('',#33849,#4093);
#2495=LINE('',#33851,#4094);
#2496=LINE('',#33855,#4095);
#2497=LINE('',#33857,#4096);
#2498=LINE('',#33859,#4097);
#2499=LINE('',#33860,#4098);
#2500=LINE('',#33863,#4099);
#2501=LINE('',#33865,#4100);
#2502=LINE('',#33866,#4101);
#2503=LINE('',#33869,#4102);
#2504=LINE('',#33871,#4103);
#2505=LINE('',#33872,#4104);
#2506=LINE('',#33874,#4105);
#2507=LINE('',#33876,#4106);
#2508=LINE('',#33878,#4107);
#2509=LINE('',#33879,#4108);
#2510=LINE('',#33881,#4109);
#2511=LINE('',#33882,#4110);
#2512=LINE('',#33883,#4111);
#2513=LINE('',#33886,#4112);
#2514=LINE('',#33889,#4113);
#2515=LINE('',#33891,#4114);
#2516=LINE('',#33893,#4115);
#2517=LINE('',#33894,#4116);
#2518=LINE('',#33897,#4117);
#2519=LINE('',#33898,#4118);
#2520=LINE('',#33901,#4119);
#2521=LINE('',#33903,#4120);
#2522=LINE('',#33904,#4121);
#2523=LINE('',#33905,#4122);
#2524=LINE('',#33908,#4123);
#2525=LINE('',#33909,#4124);
#2526=LINE('',#33911,#4125);
#2527=LINE('',#33913,#4126);
#2528=LINE('',#33915,#4127);
#2529=LINE('',#33922,#4128);
#2530=LINE('',#33928,#4129);
#2531=LINE('',#33938,#4130);
#2532=LINE('',#33941,#4131);
#2533=LINE('',#33946,#4132);
#2534=LINE('',#33952,#4133);
#2535=LINE('',#33956,#4134);
#2536=LINE('',#33958,#4135);
#2537=LINE('',#33959,#4136);
#2538=LINE('',#33965,#4137);
#2539=LINE('',#33968,#4138);
#2540=LINE('',#33973,#4139);
#2541=LINE('',#33979,#4140);
#2542=LINE('',#33983,#4141);
#2543=LINE('',#33985,#4142);
#2544=LINE('',#33986,#4143);
#2545=LINE('',#33992,#4144);
#2546=LINE('',#33995,#4145);
#2547=LINE('',#34000,#4146);
#2548=LINE('',#34006,#4147);
#2549=LINE('',#34010,#4148);
#2550=LINE('',#34012,#4149);
#2551=LINE('',#34013,#4150);
#2552=LINE('',#34019,#4151);
#2553=LINE('',#34022,#4152);
#2554=LINE('',#34027,#4153);
#2555=LINE('',#34033,#4154);
#2556=LINE('',#34037,#4155);
#2557=LINE('',#34039,#4156);
#2558=LINE('',#34040,#4157);
#2559=LINE('',#34046,#4158);
#2560=LINE('',#34049,#4159);
#2561=LINE('',#34054,#4160);
#2562=LINE('',#34060,#4161);
#2563=LINE('',#34064,#4162);
#2564=LINE('',#34066,#4163);
#2565=LINE('',#34067,#4164);
#2566=LINE('',#34070,#4165);
#2567=LINE('',#34072,#4166);
#2568=LINE('',#34073,#4167);
#2569=LINE('',#34076,#4168);
#2570=LINE('',#34078,#4169);
#2571=LINE('',#34079,#4170);
#2572=LINE('',#34082,#4171);
#2573=LINE('',#34084,#4172);
#2574=LINE('',#34085,#4173);
#2575=LINE('',#34088,#4174);
#2576=LINE('',#34090,#4175);
#2577=LINE('',#34091,#4176);
#2578=LINE('',#34096,#4177);
#2579=LINE('',#34103,#4178);
#2580=LINE('',#34107,#4179);
#2581=LINE('',#34112,#4180);
#2582=LINE('',#34117,#4181);
#2583=LINE('',#34120,#4182);
#2584=LINE('',#34123,#4183);
#2585=LINE('',#34128,#4184);
#2586=LINE('',#34129,#4185);
#2587=LINE('',#34133,#4186);
#2588=LINE('',#34135,#4187);
#2589=LINE('',#34145,#4188);
#2590=LINE('',#34148,#4189);
#2591=LINE('',#34153,#4190);
#2592=LINE('',#34159,#4191);
#2593=LINE('',#34163,#4192);
#2594=LINE('',#34165,#4193);
#2595=LINE('',#34166,#4194);
#2596=LINE('',#34172,#4195);
#2597=LINE('',#34175,#4196);
#2598=LINE('',#34180,#4197);
#2599=LINE('',#34186,#4198);
#2600=LINE('',#34190,#4199);
#2601=LINE('',#34192,#4200);
#2602=LINE('',#34193,#4201);
#2603=LINE('',#34199,#4202);
#2604=LINE('',#34202,#4203);
#2605=LINE('',#34207,#4204);
#2606=LINE('',#34213,#4205);
#2607=LINE('',#34217,#4206);
#2608=LINE('',#34219,#4207);
#2609=LINE('',#34220,#4208);
#2610=LINE('',#34226,#4209);
#2611=LINE('',#34229,#4210);
#2612=LINE('',#34234,#4211);
#2613=LINE('',#34240,#4212);
#2614=LINE('',#34244,#4213);
#2615=LINE('',#34246,#4214);
#2616=LINE('',#34247,#4215);
#2617=LINE('',#34253,#4216);
#2618=LINE('',#34256,#4217);
#2619=LINE('',#34261,#4218);
#2620=LINE('',#34267,#4219);
#2621=LINE('',#34271,#4220);
#2622=LINE('',#34273,#4221);
#2623=LINE('',#34274,#4222);
#2624=LINE('',#34277,#4223);
#2625=LINE('',#34279,#4224);
#2626=LINE('',#34280,#4225);
#2627=LINE('',#34283,#4226);
#2628=LINE('',#34285,#4227);
#2629=LINE('',#34286,#4228);
#2630=LINE('',#34289,#4229);
#2631=LINE('',#34291,#4230);
#2632=LINE('',#34292,#4231);
#2633=LINE('',#34295,#4232);
#2634=LINE('',#34297,#4233);
#2635=LINE('',#34298,#4234);
#2636=LINE('',#34303,#4235);
#2637=LINE('',#34310,#4236);
#2638=LINE('',#34314,#4237);
#2639=LINE('',#34319,#4238);
#2640=LINE('',#34324,#4239);
#2641=LINE('',#34327,#4240);
#2642=LINE('',#34330,#4241);
#2643=LINE('',#34335,#4242);
#2644=LINE('',#34336,#4243);
#2645=LINE('',#34340,#4244);
#2646=LINE('',#34342,#4245);
#2647=LINE('',#34359,#4246);
#2648=LINE('',#34372,#4247);
#2649=LINE('',#34377,#4248);
#2650=LINE('',#34379,#4249);
#2651=LINE('',#34381,#4250);
#2652=LINE('',#34382,#4251);
#2653=LINE('',#34386,#4252);
#2654=LINE('',#34388,#4253);
#2655=LINE('',#34390,#4254);
#2656=LINE('',#34391,#4255);
#2657=LINE('',#34395,#4256);
#2658=LINE('',#34399,#4257);
#2659=LINE('',#34400,#4258);
#2660=LINE('',#34403,#4259);
#2661=LINE('',#34405,#4260);
#2662=LINE('',#34406,#4261);
#2663=LINE('',#34409,#4262);
#2664=LINE('',#34410,#4263);
#2665=LINE('',#34413,#4264);
#2666=LINE('',#34414,#4265);
#2667=LINE('',#34416,#4266);
#2668=LINE('',#34424,#4267);
#2669=LINE('',#34429,#4268);
#2670=LINE('',#34650,#4269);
#2671=LINE('',#34653,#4270);
#2672=LINE('',#34669,#4271);
#2673=LINE('',#34676,#4272);
#2674=LINE('',#34682,#4273);
#2675=LINE('',#34702,#4274);
#2676=LINE('',#34716,#4275);
#2677=LINE('',#34719,#4276);
#2678=LINE('',#34754,#4277);
#2679=LINE('',#34761,#4278);
#2680=LINE('',#34766,#4279);
#2681=LINE('',#34770,#4280);
#2682=VECTOR('',#22274,0.008);
#2683=VECTOR('',#22295,0.00616666666666666);
#2684=VECTOR('',#22302,1.);
#2685=VECTOR('',#22305,1.);
#2686=VECTOR('',#22310,1.);
#2687=VECTOR('',#22317,1.);
#2688=VECTOR('',#22322,1.);
#2689=VECTOR('',#22323,1.);
#2690=VECTOR('',#22324,1.);
#2691=VECTOR('',#22329,1.);
#2692=VECTOR('',#22332,1.);
#2693=VECTOR('',#22337,1.);
#2694=VECTOR('',#22344,1.);
#2695=VECTOR('',#22349,0.999999999999999);
#2696=VECTOR('',#22350,1.);
#2697=VECTOR('',#22351,0.999999999999999);
#2698=VECTOR('',#22356,1.);
#2699=VECTOR('',#22359,1.);
#2700=VECTOR('',#22364,1.);
#2701=VECTOR('',#22371,1.);
#2702=VECTOR('',#22376,1.);
#2703=VECTOR('',#22377,1.);
#2704=VECTOR('',#22378,1.);
#2705=VECTOR('',#22383,1.);
#2706=VECTOR('',#22386,1.);
#2707=VECTOR('',#22391,1.);
#2708=VECTOR('',#22398,1.);
#2709=VECTOR('',#22403,1.);
#2710=VECTOR('',#22404,1.);
#2711=VECTOR('',#22405,1.);
#2712=VECTOR('',#22410,1.);
#2713=VECTOR('',#22413,1.);
#2714=VECTOR('',#22418,1.);
#2715=VECTOR('',#22425,1.);
#2716=VECTOR('',#22430,1.);
#2717=VECTOR('',#22431,1.);
#2718=VECTOR('',#22432,1.);
#2719=VECTOR('',#22435,1.);
#2720=VECTOR('',#22436,1.);
#2721=VECTOR('',#22437,1.);
#2722=VECTOR('',#22440,0.999999999999999);
#2723=VECTOR('',#22441,1.);
#2724=VECTOR('',#22442,0.999999999999999);
#2725=VECTOR('',#22445,1.);
#2726=VECTOR('',#22446,1.);
#2727=VECTOR('',#22447,1.);
#2728=VECTOR('',#22450,1.);
#2729=VECTOR('',#22451,1.);
#2730=VECTOR('',#22452,1.);
#2731=VECTOR('',#22457,1.);
#2732=VECTOR('',#22468,1.);
#2733=VECTOR('',#22471,1.);
#2734=VECTOR('',#22478,1.);
#2735=VECTOR('',#22485,1.);
#2736=VECTOR('',#22488,1.);
#2737=VECTOR('',#22493,1.);
#2738=VECTOR('',#22500,1.);
#2739=VECTOR('',#22503,1.);
#2740=VECTOR('',#22506,1.);
#2741=VECTOR('',#22513,1.);
#2742=VECTOR('',#22526,0.0025);
#2743=VECTOR('',#22533,0.0045);
#2744=VECTOR('',#22546,1.);
#2745=VECTOR('',#22553,1.);
#2746=VECTOR('',#22554,1.);
#2747=VECTOR('',#22555,1.);
#2748=VECTOR('',#22558,1.);
#2749=VECTOR('',#22559,1.);
#2750=VECTOR('',#22560,1.);
#2751=VECTOR('',#22563,1.);
#2752=VECTOR('',#22568,1.);
#2753=VECTOR('',#22575,1.);
#2754=VECTOR('',#22578,1.);
#2755=VECTOR('',#22579,1.);
#2756=VECTOR('',#22582,1.);
#2757=VECTOR('',#22593,1.);
#2758=VECTOR('',#22598,1.);
#2759=VECTOR('',#22599,1.);
#2760=VECTOR('',#22600,1.);
#2761=VECTOR('',#22603,1.);
#2762=VECTOR('',#22610,1.);
#2763=VECTOR('',#22613,1.);
#2764=VECTOR('',#22622,1.);
#2765=VECTOR('',#22629,1.);
#2766=VECTOR('',#22630,1.);
#2767=VECTOR('',#22631,1.);
#2768=VECTOR('',#22634,1.);
#2769=VECTOR('',#22635,1.);
#2770=VECTOR('',#22636,1.);
#2771=VECTOR('',#22639,1.);
#2772=VECTOR('',#22644,1.);
#2773=VECTOR('',#22651,1.);
#2774=VECTOR('',#22654,1.);
#2775=VECTOR('',#22655,1.);
#2776=VECTOR('',#22658,1.);
#2777=VECTOR('',#22669,1.);
#2778=VECTOR('',#22674,1.);
#2779=VECTOR('',#22675,1.);
#2780=VECTOR('',#22676,1.);
#2781=VECTOR('',#22679,1.);
#2782=VECTOR('',#22686,1.);
#2783=VECTOR('',#22689,1.);
#2784=VECTOR('',#22698,1.);
#2785=VECTOR('',#22705,1.);
#2786=VECTOR('',#22706,1.);
#2787=VECTOR('',#22707,1.);
#2788=VECTOR('',#22710,1.);
#2789=VECTOR('',#22711,1.);
#2790=VECTOR('',#22712,1.);
#2791=VECTOR('',#22715,1.);
#2792=VECTOR('',#22720,1.);
#2793=VECTOR('',#22727,1.);
#2794=VECTOR('',#22730,1.);
#2795=VECTOR('',#22731,1.);
#2796=VECTOR('',#22734,1.);
#2797=VECTOR('',#22745,1.);
#2798=VECTOR('',#22750,1.);
#2799=VECTOR('',#22751,1.);
#2800=VECTOR('',#22752,1.);
#2801=VECTOR('',#22755,1.);
#2802=VECTOR('',#22762,1.);
#2803=VECTOR('',#22765,1.);
#2804=VECTOR('',#22774,1.);
#2805=VECTOR('',#22781,1.);
#2806=VECTOR('',#22782,1.);
#2807=VECTOR('',#22783,1.);
#2808=VECTOR('',#22786,1.);
#2809=VECTOR('',#22787,1.);
#2810=VECTOR('',#22788,1.);
#2811=VECTOR('',#22791,1.);
#2812=VECTOR('',#22796,1.);
#2813=VECTOR('',#22803,1.);
#2814=VECTOR('',#22806,1.);
#2815=VECTOR('',#22807,1.);
#2816=VECTOR('',#22810,1.);
#2817=VECTOR('',#22821,1.);
#2818=VECTOR('',#22826,1.);
#2819=VECTOR('',#22827,1.);
#2820=VECTOR('',#22828,1.);
#2821=VECTOR('',#22831,1.);
#2822=VECTOR('',#22838,1.);
#2823=VECTOR('',#22841,1.);
#2824=VECTOR('',#22850,1.);
#2825=VECTOR('',#22857,1.);
#2826=VECTOR('',#22858,1.);
#2827=VECTOR('',#22859,1.);
#2828=VECTOR('',#22862,1.);
#2829=VECTOR('',#22863,1.);
#2830=VECTOR('',#22864,1.);
#2831=VECTOR('',#22867,1.);
#2832=VECTOR('',#22872,1.);
#2833=VECTOR('',#22879,1.);
#2834=VECTOR('',#22882,1.);
#2835=VECTOR('',#22883,1.);
#2836=VECTOR('',#22886,1.);
#2837=VECTOR('',#22897,1.);
#2838=VECTOR('',#22902,1.);
#2839=VECTOR('',#22903,1.);
#2840=VECTOR('',#22904,1.);
#2841=VECTOR('',#22907,1.);
#2842=VECTOR('',#22914,1.);
#2843=VECTOR('',#22917,1.);
#2844=VECTOR('',#22926,1.);
#2845=VECTOR('',#22933,1.);
#2846=VECTOR('',#22934,1.);
#2847=VECTOR('',#22935,1.);
#2848=VECTOR('',#22938,1.);
#2849=VECTOR('',#22939,1.);
#2850=VECTOR('',#22940,1.);
#2851=VECTOR('',#22943,1.);
#2852=VECTOR('',#22948,1.);
#2853=VECTOR('',#22955,1.);
#2854=VECTOR('',#22958,1.);
#2855=VECTOR('',#22959,1.);
#2856=VECTOR('',#22962,1.);
#2857=VECTOR('',#22973,1.);
#2858=VECTOR('',#22978,1.);
#2859=VECTOR('',#22979,1.);
#2860=VECTOR('',#22980,1.);
#2861=VECTOR('',#22983,1.);
#2862=VECTOR('',#22990,1.);
#2863=VECTOR('',#22993,1.);
#2864=VECTOR('',#23002,1.);
#2865=VECTOR('',#23009,1.);
#2866=VECTOR('',#23010,1.);
#2867=VECTOR('',#23011,1.);
#2868=VECTOR('',#23014,1.);
#2869=VECTOR('',#23015,1.);
#2870=VECTOR('',#23016,1.);
#2871=VECTOR('',#23019,1.);
#2872=VECTOR('',#23024,1.);
#2873=VECTOR('',#23031,1.);
#2874=VECTOR('',#23034,1.);
#2875=VECTOR('',#23035,1.);
#2876=VECTOR('',#23038,1.);
#2877=VECTOR('',#23049,1.);
#2878=VECTOR('',#23054,1.);
#2879=VECTOR('',#23055,1.);
#2880=VECTOR('',#23056,1.);
#2881=VECTOR('',#23059,1.);
#2882=VECTOR('',#23066,1.);
#2883=VECTOR('',#23069,1.);
#2884=VECTOR('',#23078,1.);
#2885=VECTOR('',#23085,1.);
#2886=VECTOR('',#23086,1.);
#2887=VECTOR('',#23087,1.);
#2888=VECTOR('',#23090,1.);
#2889=VECTOR('',#23091,1.);
#2890=VECTOR('',#23092,1.);
#2891=VECTOR('',#23095,1.);
#2892=VECTOR('',#23100,1.);
#2893=VECTOR('',#23107,1.);
#2894=VECTOR('',#23110,1.);
#2895=VECTOR('',#23111,1.);
#2896=VECTOR('',#23114,1.);
#2897=VECTOR('',#23125,1.);
#2898=VECTOR('',#23130,1.);
#2899=VECTOR('',#23131,1.);
#2900=VECTOR('',#23132,1.);
#2901=VECTOR('',#23135,1.);
#2902=VECTOR('',#23146,1.);
#2903=VECTOR('',#23149,1.);
#2904=VECTOR('',#23152,1.);
#2905=VECTOR('',#23153,1.);
#2906=VECTOR('',#23154,1.);
#2907=VECTOR('',#23155,1.);
#2908=VECTOR('',#23156,1.);
#2909=VECTOR('',#23157,1.);
#2910=VECTOR('',#23158,1.);
#2911=VECTOR('',#23159,1.);
#2912=VECTOR('',#23160,1.);
#2913=VECTOR('',#23161,1.);
#2914=VECTOR('',#23162,1.);
#2915=VECTOR('',#23163,1.);
#2916=VECTOR('',#23164,1.);
#2917=VECTOR('',#23165,1.);
#2918=VECTOR('',#23166,1.);
#2919=VECTOR('',#23167,1.);
#2920=VECTOR('',#23170,1.);
#2921=VECTOR('',#23171,1.);
#2922=VECTOR('',#23172,1.);
#2923=VECTOR('',#23175,1.);
#2924=VECTOR('',#23176,1.);
#2925=VECTOR('',#23179,1.);
#2926=VECTOR('',#23180,1.);
#2927=VECTOR('',#23181,1.);
#2928=VECTOR('',#23184,1.);
#2929=VECTOR('',#23185,1.);
#2930=VECTOR('',#23186,1.);
#2931=VECTOR('',#23187,1.);
#2932=VECTOR('',#23190,1.);
#2933=VECTOR('',#23191,1.);
#2934=VECTOR('',#23194,1.);
#2935=VECTOR('',#23195,1.);
#2936=VECTOR('',#23198,1.);
#2937=VECTOR('',#23201,1.);
#2938=VECTOR('',#23202,1.);
#2939=VECTOR('',#23203,1.);
#2940=VECTOR('',#23204,1.);
#2941=VECTOR('',#23205,1.);
#2942=VECTOR('',#23206,1.);
#2943=VECTOR('',#23207,1.);
#2944=VECTOR('',#23208,1.);
#2945=VECTOR('',#23209,1.);
#2946=VECTOR('',#23210,1.);
#2947=VECTOR('',#23211,1.);
#2948=VECTOR('',#23212,1.);
#2949=VECTOR('',#23213,1.);
#2950=VECTOR('',#23214,1.);
#2951=VECTOR('',#23215,1.);
#2952=VECTOR('',#23218,1.);
#2953=VECTOR('',#23219,1.);
#2954=VECTOR('',#23222,1.);
#2955=VECTOR('',#23225,1.);
#2956=VECTOR('',#23228,1.);
#2957=VECTOR('',#23231,1.);
#2958=VECTOR('',#23234,1.);
#2959=VECTOR('',#23237,1.);
#2960=VECTOR('',#23240,1.);
#2961=VECTOR('',#23241,1.);
#2962=VECTOR('',#23242,1.);
#2963=VECTOR('',#23243,1.);
#2964=VECTOR('',#23244,1.);
#2965=VECTOR('',#23245,1.);
#2966=VECTOR('',#23248,1.);
#2967=VECTOR('',#23249,1.);
#2968=VECTOR('',#23250,1.);
#2969=VECTOR('',#23251,1.);
#2970=VECTOR('',#23252,1.);
#2971=VECTOR('',#23255,1.);
#2972=VECTOR('',#23256,1.);
#2973=VECTOR('',#23257,1.);
#2974=VECTOR('',#23258,1.);
#2975=VECTOR('',#23259,1.);
#2976=VECTOR('',#23264,1.);
#2977=VECTOR('',#23265,1.);
#2978=VECTOR('',#23266,1.);
#2979=VECTOR('',#23267,1.);
#2980=VECTOR('',#23268,1.);
#2981=VECTOR('',#23271,1.);
#2982=VECTOR('',#23272,1.);
#2983=VECTOR('',#23275,1.);
#2984=VECTOR('',#23276,1.);
#2985=VECTOR('',#23287,1.);
#2986=VECTOR('',#23294,1.);
#2987=VECTOR('',#23297,1.);
#2988=VECTOR('',#23302,1.);
#2989=VECTOR('',#23305,1.);
#2990=VECTOR('',#23310,1.);
#2991=VECTOR('',#23313,1.);
#2992=VECTOR('',#23318,1.);
#2993=VECTOR('',#23321,1.);
#2994=VECTOR('',#23326,1.);
#2995=VECTOR('',#23329,1.);
#2996=VECTOR('',#23334,1.);
#2997=VECTOR('',#23337,1.);
#2998=VECTOR('',#23342,1.);
#2999=VECTOR('',#23345,1.);
#3000=VECTOR('',#23350,1.);
#3001=VECTOR('',#23353,1.);
#3002=VECTOR('',#23358,1.);
#3003=VECTOR('',#23361,1.);
#3004=VECTOR('',#23366,1.);
#3005=VECTOR('',#23369,1.);
#3006=VECTOR('',#23374,1.);
#3007=VECTOR('',#23377,1.);
#3008=VECTOR('',#23382,1.);
#3009=VECTOR('',#23385,1.);
#3010=VECTOR('',#23390,1.);
#3011=VECTOR('',#23393,1.);
#3012=VECTOR('',#23398,1.);
#3013=VECTOR('',#23401,1.);
#3014=VECTOR('',#23406,1.);
#3015=VECTOR('',#23409,1.);
#3016=VECTOR('',#23414,1.);
#3017=VECTOR('',#23417,1.);
#3018=VECTOR('',#23422,1.);
#3019=VECTOR('',#23425,1.);
#3020=VECTOR('',#23430,1.);
#3021=VECTOR('',#23433,1.);
#3022=VECTOR('',#23438,1.);
#3023=VECTOR('',#23441,1.);
#3024=VECTOR('',#23446,1.);
#3025=VECTOR('',#23449,1.);
#3026=VECTOR('',#23454,1.);
#3027=VECTOR('',#23457,1.);
#3028=VECTOR('',#23462,1.);
#3029=VECTOR('',#23465,1.);
#3030=VECTOR('',#23470,1.);
#3031=VECTOR('',#23473,1.);
#3032=VECTOR('',#23478,1.);
#3033=VECTOR('',#23481,1.);
#3034=VECTOR('',#23486,1.);
#3035=VECTOR('',#23489,1.);
#3036=VECTOR('',#23494,1.);
#3037=VECTOR('',#23497,1.);
#3038=VECTOR('',#23502,1.);
#3039=VECTOR('',#23505,1.);
#3040=VECTOR('',#23510,1.);
#3041=VECTOR('',#23513,1.);
#3042=VECTOR('',#23518,1.);
#3043=VECTOR('',#23521,1.);
#3044=VECTOR('',#23526,1.);
#3045=VECTOR('',#23529,1.);
#3046=VECTOR('',#23534,1.);
#3047=VECTOR('',#23537,1.);
#3048=VECTOR('',#23542,1.);
#3049=VECTOR('',#23545,1.);
#3050=VECTOR('',#23550,1.);
#3051=VECTOR('',#23553,1.);
#3052=VECTOR('',#23558,1.);
#3053=VECTOR('',#23561,1.);
#3054=VECTOR('',#23566,1.);
#3055=VECTOR('',#23569,1.);
#3056=VECTOR('',#23574,1.);
#3057=VECTOR('',#23577,1.);
#3058=VECTOR('',#23582,1.);
#3059=VECTOR('',#23585,1.);
#3060=VECTOR('',#23590,1.);
#3061=VECTOR('',#23593,1.);
#3062=VECTOR('',#23598,1.);
#3063=VECTOR('',#23601,1.);
#3064=VECTOR('',#23606,1.);
#3065=VECTOR('',#23609,1.);
#3066=VECTOR('',#23614,1.);
#3067=VECTOR('',#23617,1.);
#3068=VECTOR('',#23622,1.);
#3069=VECTOR('',#23625,1.);
#3070=VECTOR('',#23630,1.);
#3071=VECTOR('',#23633,1.);
#3072=VECTOR('',#23638,1.);
#3073=VECTOR('',#23641,1.);
#3074=VECTOR('',#23744,1.);
#3075=VECTOR('',#23747,1.);
#3076=VECTOR('',#23932,0.0025);
#3077=VECTOR('',#23937,0.01);
#3078=VECTOR('',#23938,0.01);
#3079=VECTOR('',#23939,0.01);
#3080=VECTOR('',#23940,0.01);
#3081=VECTOR('',#23947,0.01);
#3082=VECTOR('',#23956,0.01);
#3083=VECTOR('',#23969,0.01);
#3084=VECTOR('',#23974,0.01);
#3085=VECTOR('',#23975,0.01);
#3086=VECTOR('',#23976,0.01);
#3087=VECTOR('',#23983,0.01);
#3088=VECTOR('',#23992,0.01);
#3089=VECTOR('',#24005,0.01);
#3090=VECTOR('',#24010,0.01);
#3091=VECTOR('',#24011,0.01);
#3092=VECTOR('',#24012,0.01);
#3093=VECTOR('',#24019,0.01);
#3094=VECTOR('',#24028,0.01);
#3095=VECTOR('',#24037,0.01);
#3096=VECTOR('',#24038,0.01);
#3097=VECTOR('',#24039,0.01);
#3098=VECTOR('',#24040,0.01);
#3099=VECTOR('',#24043,0.01);
#3100=VECTOR('',#24044,0.01);
#3101=VECTOR('',#24045,0.01);
#3102=VECTOR('',#24046,0.01);
#3103=VECTOR('',#24049,0.01);
#3104=VECTOR('',#24050,0.01);
#3105=VECTOR('',#24051,0.01);
#3106=VECTOR('',#24052,0.01);
#3107=VECTOR('',#24055,0.01);
#3108=VECTOR('',#24056,0.01);
#3109=VECTOR('',#24057,0.01);
#3110=VECTOR('',#24058,0.01);
#3111=VECTOR('',#24067,0.01);
#3112=VECTOR('',#24080,0.01);
#3113=VECTOR('',#24093,0.01);
#3114=VECTOR('',#24100,0.01);
#3115=VECTOR('',#24101,0.01);
#3116=VECTOR('',#24102,0.01);
#3117=VECTOR('',#24105,0.01);
#3118=VECTOR('',#24106,0.01);
#3119=VECTOR('',#24107,0.01);
#3120=VECTOR('',#24108,0.01);
#3121=VECTOR('',#24111,1.);
#3122=VECTOR('',#24116,0.003125);
#3123=VECTOR('',#24125,1.);
#3124=VECTOR('',#24128,1.);
#3125=VECTOR('',#24133,0.003125);
#3126=VECTOR('',#24142,1.);
#3127=VECTOR('',#24145,1.);
#3128=VECTOR('',#24150,0.003125);
#3129=VECTOR('',#24159,1.);
#3130=VECTOR('',#24160,1.);
#3131=VECTOR('',#24161,1.);
#3132=VECTOR('',#24164,1.);
#3133=VECTOR('',#24165,1.);
#3134=VECTOR('',#24166,1.);
#3135=VECTOR('',#24169,1.);
#3136=VECTOR('',#24170,1.);
#3137=VECTOR('',#24171,1.);
#3138=VECTOR('',#24174,1.);
#3139=VECTOR('',#24175,1.);
#3140=VECTOR('',#24176,1.);
#3141=VECTOR('',#24179,1.);
#3142=VECTOR('',#24180,1.);
#3143=VECTOR('',#24181,1.);
#3144=VECTOR('',#24182,1.);
#3145=VECTOR('',#24193,0.003);
#3146=VECTOR('',#24198,0.003);
#3147=VECTOR('',#24203,0.003125);
#3148=VECTOR('',#24210,0.003);
#3149=VECTOR('',#24215,0.003);
#3150=VECTOR('',#24220,1.);
#3151=VECTOR('',#24223,1.);
#3152=VECTOR('',#24226,1.);
#3153=VECTOR('',#24227,1.);
#3154=VECTOR('',#24228,1.);
#3155=VECTOR('',#24231,1.);
#3156=VECTOR('',#24232,1.);
#3157=VECTOR('',#24233,1.);
#3158=VECTOR('',#24234,1.);
#3159=VECTOR('',#24235,1.);
#3160=VECTOR('',#24236,1.);
#3161=VECTOR('',#24237,1.);
#3162=VECTOR('',#24240,1.);
#3163=VECTOR('',#24251,1.);
#3164=VECTOR('',#24254,1.);
#3165=VECTOR('',#24257,1.);
#3166=VECTOR('',#24258,1.);
#3167=VECTOR('',#24259,1.);
#3168=VECTOR('',#24260,1.);
#3169=VECTOR('',#24261,1.);
#3170=VECTOR('',#24262,1.);
#3171=VECTOR('',#24265,1.);
#3172=VECTOR('',#24266,1.);
#3173=VECTOR('',#24269,1.);
#3174=VECTOR('',#24270,1.);
#3175=VECTOR('',#24273,1.);
#3176=VECTOR('',#24274,1.);
#3177=VECTOR('',#24277,1.);
#3178=VECTOR('',#24278,1.);
#3179=VECTOR('',#24281,1.);
#3180=VECTOR('',#24284,1.);
#3181=VECTOR('',#24285,1.);
#3182=VECTOR('',#24286,1.);
#3183=VECTOR('',#24291,1.);
#3184=VECTOR('',#24294,1.);
#3185=VECTOR('',#24297,1.);
#3186=VECTOR('',#24298,1.);
#3187=VECTOR('',#24299,1.);
#3188=VECTOR('',#24304,1.);
#3189=VECTOR('',#24309,1.);
#3190=VECTOR('',#24310,1.);
#3191=VECTOR('',#24311,1.);
#3192=VECTOR('',#24316,1.);
#3193=VECTOR('',#24321,1.);
#3194=VECTOR('',#24322,1.);
#3195=VECTOR('',#24323,1.);
#3196=VECTOR('',#24328,1.);
#3197=VECTOR('',#24333,1.);
#3198=VECTOR('',#24336,1.);
#3199=VECTOR('',#24341,1.);
#3200=VECTOR('',#24346,0.0045);
#3201=VECTOR('',#24349,1.);
#3202=VECTOR('',#24350,1.);
#3203=VECTOR('',#24353,1.);
#3204=VECTOR('',#24358,1.);
#3205=VECTOR('',#24361,1.);
#3206=VECTOR('',#24364,1.);
#3207=VECTOR('',#24377,1.);
#3208=VECTOR('',#24380,1.);
#3209=VECTOR('',#24383,1.);
#3210=VECTOR('',#24386,1.);
#3211=VECTOR('',#24387,1.);
#3212=VECTOR('',#24388,1.);
#3213=VECTOR('',#24391,1.);
#3214=VECTOR('',#24392,1.);
#3215=VECTOR('',#24393,1.);
#3216=VECTOR('',#24394,1.);
#3217=VECTOR('',#24399,1.);
#3218=VECTOR('',#24402,1.);
#3219=VECTOR('',#24405,1.);
#3220=VECTOR('',#24408,1.);
#3221=VECTOR('',#24409,1.);
#3222=VECTOR('',#24410,1.);
#3223=VECTOR('',#24411,1.);
#3224=VECTOR('',#24418,0.012875);
#3225=VECTOR('',#24429,0.013);
#3226=VECTOR('',#24434,0.008125);
#3227=VECTOR('',#24439,0.008);
#3228=VECTOR('',#24448,0.0017);
#3229=VECTOR('',#24455,0.0017);
#3230=VECTOR('',#24462,0.0017);
#3231=VECTOR('',#24469,0.0017);
#3232=VECTOR('',#24472,1.);
#3233=VECTOR('',#24473,1.);
#3234=VECTOR('',#24474,1.);
#3235=VECTOR('',#24479,0.006);
#3236=VECTOR('',#24508,0.008);
#3237=VECTOR('',#24529,0.00616666666666666);
#3238=VECTOR('',#24534,1.);
#3239=VECTOR('',#24535,1.);
#3240=VECTOR('',#24536,1.);
#3241=VECTOR('',#24537,1.);
#3242=VECTOR('',#24540,1.);
#3243=VECTOR('',#24541,1.);
#3244=VECTOR('',#24542,1.);
#3245=VECTOR('',#24545,1.);
#3246=VECTOR('',#24548,1.);
#3247=VECTOR('',#24553,1.);
#3248=VECTOR('',#24554,1.);
#3249=VECTOR('',#24557,1.);
#3250=VECTOR('',#24558,1.);
#3251=VECTOR('',#24559,1.);
#3252=VECTOR('',#24562,1.);
#3253=VECTOR('',#24563,1.);
#3254=VECTOR('',#24566,1.);
#3255=VECTOR('',#24567,1.);
#3256=VECTOR('',#24570,1.);
#3257=VECTOR('',#24577,1.);
#3258=VECTOR('',#24578,1.);
#3259=VECTOR('',#24579,1.);
#3260=VECTOR('',#24580,1.);
#3261=VECTOR('',#24585,1.);
#3262=VECTOR('',#24586,1.);
#3263=VECTOR('',#24587,1.);
#3264=VECTOR('',#24588,1.);
#3265=VECTOR('',#24589,1.);
#3266=VECTOR('',#24592,1.);
#3267=VECTOR('',#24597,1.);
#3268=VECTOR('',#24598,1.);
#3269=VECTOR('',#24599,1.);
#3270=VECTOR('',#24600,1.);
#3271=VECTOR('',#24601,1.);
#3272=VECTOR('',#24604,1.);
#3273=VECTOR('',#24607,1.);
#3274=VECTOR('',#24610,1.);
#3275=VECTOR('',#24613,1.);
#3276=VECTOR('',#24622,1.);
#3277=VECTOR('',#24625,1.);
#3278=VECTOR('',#24630,1.);
#3279=VECTOR('',#24635,1.);
#3280=VECTOR('',#24636,1.);
#3281=VECTOR('',#24637,1.);
#3282=VECTOR('',#24642,1.);
#3283=VECTOR('',#24649,1.);
#3284=VECTOR('',#24654,1.);
#3285=VECTOR('',#24655,1.);
#3286=VECTOR('',#24656,1.);
#3287=VECTOR('',#24661,1.);
#3288=VECTOR('',#24668,1.);
#3289=VECTOR('',#24675,1.);
#3290=VECTOR('',#24680,1.);
#3291=VECTOR('',#24681,1.);
#3292=VECTOR('',#24682,1.);
#3293=VECTOR('',#24687,1.);
#3294=VECTOR('',#24692,1.);
#3295=VECTOR('',#24693,1.);
#3296=VECTOR('',#24694,1.);
#3297=VECTOR('',#24699,1.);
#3298=VECTOR('',#24706,1.);
#3299=VECTOR('',#24713,1.);
#3300=VECTOR('',#24718,1.);
#3301=VECTOR('',#24719,1.);
#3302=VECTOR('',#24720,1.);
#3303=VECTOR('',#24725,1.);
#3304=VECTOR('',#24732,1.);
#3305=VECTOR('',#24737,1.);
#3306=VECTOR('',#24738,1.);
#3307=VECTOR('',#24739,1.);
#3308=VECTOR('',#24756,1.);
#3309=VECTOR('',#24759,1.);
#3310=VECTOR('',#24764,1.);
#3311=VECTOR('',#24771,1.);
#3312=VECTOR('',#24776,1.);
#3313=VECTOR('',#24777,1.);
#3314=VECTOR('',#24778,1.);
#3315=VECTOR('',#24783,1.);
#3316=VECTOR('',#24786,1.);
#3317=VECTOR('',#24791,1.);
#3318=VECTOR('',#24798,1.);
#3319=VECTOR('',#24803,1.);
#3320=VECTOR('',#24804,1.);
#3321=VECTOR('',#24805,1.);
#3322=VECTOR('',#24810,1.);
#3323=VECTOR('',#24813,1.);
#3324=VECTOR('',#24818,1.);
#3325=VECTOR('',#24825,1.);
#3326=VECTOR('',#24830,1.);
#3327=VECTOR('',#24831,1.);
#3328=VECTOR('',#24832,1.);
#3329=VECTOR('',#24837,1.);
#3330=VECTOR('',#24840,1.);
#3331=VECTOR('',#24845,1.);
#3332=VECTOR('',#24852,1.);
#3333=VECTOR('',#24857,1.);
#3334=VECTOR('',#24858,1.);
#3335=VECTOR('',#24859,1.);
#3336=VECTOR('',#24864,1.);
#3337=VECTOR('',#24867,1.);
#3338=VECTOR('',#24872,1.);
#3339=VECTOR('',#24879,1.);
#3340=VECTOR('',#24884,1.);
#3341=VECTOR('',#24885,1.);
#3342=VECTOR('',#24886,1.);
#3343=VECTOR('',#24889,1.);
#3344=VECTOR('',#24890,1.);
#3345=VECTOR('',#24891,1.);
#3346=VECTOR('',#24894,1.);
#3347=VECTOR('',#24895,1.);
#3348=VECTOR('',#24896,1.);
#3349=VECTOR('',#24899,1.);
#3350=VECTOR('',#24900,1.);
#3351=VECTOR('',#24901,1.);
#3352=VECTOR('',#24904,1.);
#3353=VECTOR('',#24905,1.);
#3354=VECTOR('',#24906,1.);
#3355=VECTOR('',#24911,1.);
#3356=VECTOR('',#24922,1.);
#3357=VECTOR('',#24925,1.);
#3358=VECTOR('',#24932,1.);
#3359=VECTOR('',#24939,1.);
#3360=VECTOR('',#24942,1.);
#3361=VECTOR('',#24947,1.);
#3362=VECTOR('',#24954,1.);
#3363=VECTOR('',#24955,1.);
#3364=VECTOR('',#24960,1.);
#3365=VECTOR('',#24963,1.);
#3366=VECTOR('',#24976,0.01);
#3367=VECTOR('',#24985,0.01);
#3368=VECTOR('',#24996,0.01);
#3369=VECTOR('',#25005,0.01);
#3370=VECTOR('',#25016,0.01);
#3371=VECTOR('',#25025,0.01);
#3372=VECTOR('',#25036,0.01);
#3373=VECTOR('',#25045,0.01);
#3374=VECTOR('',#25086,1.);
#3375=VECTOR('',#25087,1.);
#3376=VECTOR('',#25090,1.);
#3377=VECTOR('',#25093,1.);
#3378=VECTOR('',#25094,1.);
#3379=VECTOR('',#25097,1.);
#3380=VECTOR('',#25100,1.);
#3381=VECTOR('',#25101,1.);
#3382=VECTOR('',#25104,1.);
#3383=VECTOR('',#25105,1.);
#3384=VECTOR('',#25106,1.);
#3385=VECTOR('',#25107,1.);
#3386=VECTOR('',#25108,1.);
#3387=VECTOR('',#25109,1.);
#3388=VECTOR('',#25110,1.);
#3389=VECTOR('',#25111,1.);
#3390=VECTOR('',#25112,1.);
#3391=VECTOR('',#25123,1.);
#3392=VECTOR('',#25126,1.);
#3393=VECTOR('',#25139,1.);
#3394=VECTOR('',#25140,1.);
#3395=VECTOR('',#25141,1.);
#3396=VECTOR('',#25142,1.);
#3397=VECTOR('',#25145,1.);
#3398=VECTOR('',#25146,1.);
#3399=VECTOR('',#25147,1.);
#3400=VECTOR('',#25150,1.);
#3401=VECTOR('',#25151,1.);
#3402=VECTOR('',#25152,1.);
#3403=VECTOR('',#25155,1.);
#3404=VECTOR('',#25156,1.);
#3405=VECTOR('',#25157,1.);
#3406=VECTOR('',#25160,1.);
#3407=VECTOR('',#25161,1.);
#3408=VECTOR('',#25162,1.);
#3409=VECTOR('',#25165,1.);
#3410=VECTOR('',#25166,1.);
#3411=VECTOR('',#25167,1.);
#3412=VECTOR('',#25170,1.);
#3413=VECTOR('',#25171,1.);
#3414=VECTOR('',#25172,1.);
#3415=VECTOR('',#25175,1.);
#3416=VECTOR('',#25176,1.);
#3417=VECTOR('',#25179,1.);
#3418=VECTOR('',#25180,1.);
#3419=VECTOR('',#25183,1.);
#3420=VECTOR('',#25186,1.);
#3421=VECTOR('',#25189,1.);
#3422=VECTOR('',#25196,1.);
#3423=VECTOR('',#25201,0.010775);
#3424=VECTOR('',#25212,0.0109);
#3425=VECTOR('',#25217,0.004625);
#3426=VECTOR('',#25224,0.0045);
#3427=VECTOR('',#25227,0.004625);
#3428=VECTOR('',#25238,0.012875);
#3429=VECTOR('',#25247,0.013);
#3430=VECTOR('',#25252,0.008125);
#3431=VECTOR('',#25257,0.008);
#3432=VECTOR('',#25262,0.0012295);
#3433=VECTOR('',#25265,0.0012295);
#3434=VECTOR('',#25268,0.0012295);
#3435=VECTOR('',#25271,0.0012295);
#3436=VECTOR('',#25276,0.006);
#3437=VECTOR('',#25281,1.);
#3438=VECTOR('',#25284,1.);
#3439=VECTOR('',#25287,1.);
#3440=VECTOR('',#25298,1.);
#3441=VECTOR('',#25301,1.);
#3442=VECTOR('',#25306,1.);
#3443=VECTOR('',#25313,1.);
#3444=VECTOR('',#25318,1.);
#3445=VECTOR('',#25319,1.);
#3446=VECTOR('',#25320,1.);
#3447=VECTOR('',#25325,1.);
#3448=VECTOR('',#25328,1.);
#3449=VECTOR('',#25333,1.);
#3450=VECTOR('',#25340,1.);
#3451=VECTOR('',#25345,1.);
#3452=VECTOR('',#25346,1.);
#3453=VECTOR('',#25347,1.);
#3454=VECTOR('',#25352,1.);
#3455=VECTOR('',#25355,1.);
#3456=VECTOR('',#25360,1.);
#3457=VECTOR('',#25367,1.);
#3458=VECTOR('',#25372,1.);
#3459=VECTOR('',#25373,1.);
#3460=VECTOR('',#25374,1.);
#3461=VECTOR('',#25379,1.);
#3462=VECTOR('',#25382,1.);
#3463=VECTOR('',#25387,1.);
#3464=VECTOR('',#25394,1.);
#3465=VECTOR('',#25399,1.);
#3466=VECTOR('',#25400,1.);
#3467=VECTOR('',#25401,1.);
#3468=VECTOR('',#25406,1.);
#3469=VECTOR('',#25409,1.);
#3470=VECTOR('',#25414,1.);
#3471=VECTOR('',#25421,1.);
#3472=VECTOR('',#25426,1.);
#3473=VECTOR('',#25427,1.);
#3474=VECTOR('',#25428,1.);
#3475=VECTOR('',#25431,1.);
#3476=VECTOR('',#25432,1.);
#3477=VECTOR('',#25433,1.);
#3478=VECTOR('',#25436,1.);
#3479=VECTOR('',#25437,1.);
#3480=VECTOR('',#25438,1.);
#3481=VECTOR('',#25441,1.);
#3482=VECTOR('',#25442,1.);
#3483=VECTOR('',#25443,1.);
#3484=VECTOR('',#25446,1.);
#3485=VECTOR('',#25447,1.);
#3486=VECTOR('',#25448,1.);
#3487=VECTOR('',#25453,1.);
#3488=VECTOR('',#25464,1.);
#3489=VECTOR('',#25467,1.);
#3490=VECTOR('',#25474,1.);
#3491=VECTOR('',#25481,1.);
#3492=VECTOR('',#25484,1.);
#3493=VECTOR('',#25489,1.);
#3494=VECTOR('',#25496,1.);
#3495=VECTOR('',#25497,1.);
#3496=VECTOR('',#25502,1.);
#3497=VECTOR('',#25505,1.);
#3498=VECTOR('',#25516,0.00225);
#3499=VECTOR('',#25533,0.002);
#3500=VECTOR('',#25546,1.);
#3501=VECTOR('',#25547,0.0025);
#3502=VECTOR('',#25548,1.);
#3503=VECTOR('',#25553,1.);
#3504=VECTOR('',#25558,0.0025);
#3505=VECTOR('',#25565,0.00225);
#3506=VECTOR('',#25576,0.01);
#3507=VECTOR('',#25577,0.01);
#3508=VECTOR('',#25578,0.01);
#3509=VECTOR('',#25579,0.01);
#3510=VECTOR('',#25582,0.01);
#3511=VECTOR('',#25583,0.01);
#3512=VECTOR('',#25584,0.01);
#3513=VECTOR('',#25585,0.01);
#3514=VECTOR('',#25588,0.01);
#3515=VECTOR('',#25589,0.01);
#3516=VECTOR('',#25590,0.01);
#3517=VECTOR('',#25593,0.01);
#3518=VECTOR('',#25594,0.01);
#3519=VECTOR('',#25595,0.01);
#3520=VECTOR('',#25598,1.);
#3521=VECTOR('',#25599,1.);
#3522=VECTOR('',#25600,1.);
#3523=VECTOR('',#25603,1.);
#3524=VECTOR('',#25604,1.);
#3525=VECTOR('',#25605,1.);
#3526=VECTOR('',#25606,1.);
#3527=VECTOR('',#25607,1.);
#3528=VECTOR('',#25610,1.);
#3529=VECTOR('',#25611,1.);
#3530=VECTOR('',#25612,1.);
#3531=VECTOR('',#25615,1.);
#3532=VECTOR('',#25616,1.);
#3533=VECTOR('',#25619,1.);
#3534=VECTOR('',#25620,1.);
#3535=VECTOR('',#25621,1.);
#3536=VECTOR('',#25624,1.);
#3537=VECTOR('',#25625,1.);
#3538=VECTOR('',#25628,1.);
#3539=VECTOR('',#25631,1.);
#3540=VECTOR('',#25636,1.);
#3541=VECTOR('',#25639,1.);
#3542=VECTOR('',#25640,1.);
#3543=VECTOR('',#25643,1.);
#3544=VECTOR('',#25644,1.);
#3545=VECTOR('',#25647,1.);
#3546=VECTOR('',#25656,0.00075);
#3547=VECTOR('',#25663,0.00075);
#3548=VECTOR('',#25670,0.00075);
#3549=VECTOR('',#25677,0.00075);
#3550=VECTOR('',#25684,0.0006);
#3551=VECTOR('',#25691,0.0006);
#3552=VECTOR('',#25698,0.0006);
#3553=VECTOR('',#25705,0.0006);
#3554=VECTOR('',#25712,0.0006);
#3555=VECTOR('',#25719,0.0006);
#3556=VECTOR('',#25724,1.);
#3557=VECTOR('',#25725,1.);
#3558=VECTOR('',#25726,1.);
#3559=VECTOR('',#25727,1.);
#3560=VECTOR('',#25730,1.);
#3561=VECTOR('',#25731,1.);
#3562=VECTOR('',#25732,1.);
#3563=VECTOR('',#25735,1.);
#3564=VECTOR('',#25736,1.);
#3565=VECTOR('',#25737,1.);
#3566=VECTOR('',#25738,1.);
#3567=VECTOR('',#25741,1.);
#3568=VECTOR('',#25742,1.);
#3569=VECTOR('',#25745,1.);
#3570=VECTOR('',#25746,1.);
#3571=VECTOR('',#25747,1.);
#3572=VECTOR('',#25748,1.);
#3573=VECTOR('',#25751,1.);
#3574=VECTOR('',#25752,1.);
#3575=VECTOR('',#25753,1.);
#3576=VECTOR('',#25756,1.);
#3577=VECTOR('',#25757,1.);
#3578=VECTOR('',#25764,1.);
#3579=VECTOR('',#25767,1.);
#3580=VECTOR('',#25768,1.);
#3581=VECTOR('',#25769,1.);
#3582=VECTOR('',#25772,1.);
#3583=VECTOR('',#25773,1.);
#3584=VECTOR('',#25782,1.);
#3585=VECTOR('',#25783,1.);
#3586=VECTOR('',#25784,1.);
#3587=VECTOR('',#25785,1.);
#3588=VECTOR('',#25788,1.);
#3589=VECTOR('',#25789,1.);
#3590=VECTOR('',#25790,1.);
#3591=VECTOR('',#25793,1.);
#3592=VECTOR('',#25796,1.);
#3593=VECTOR('',#25801,1.);
#3594=VECTOR('',#25802,1.);
#3595=VECTOR('',#25805,1.);
#3596=VECTOR('',#25806,1.);
#3597=VECTOR('',#25807,1.);
#3598=VECTOR('',#25810,1.);
#3599=VECTOR('',#25811,1.);
#3600=VECTOR('',#25814,1.);
#3601=VECTOR('',#25815,1.);
#3602=VECTOR('',#25818,1.);
#3603=VECTOR('',#25827,1.);
#3604=VECTOR('',#25830,1.);
#3605=VECTOR('',#25835,1.);
#3606=VECTOR('',#25842,1.);
#3607=VECTOR('',#25847,1.);
#3608=VECTOR('',#25848,1.);
#3609=VECTOR('',#25849,1.);
#3610=VECTOR('',#25854,1.);
#3611=VECTOR('',#25857,1.);
#3612=VECTOR('',#25862,1.);
#3613=VECTOR('',#25869,1.);
#3614=VECTOR('',#25874,0.999999999999999);
#3615=VECTOR('',#25875,1.);
#3616=VECTOR('',#25876,0.999999999999999);
#3617=VECTOR('',#25881,1.);
#3618=VECTOR('',#25884,1.);
#3619=VECTOR('',#25889,1.);
#3620=VECTOR('',#25896,1.);
#3621=VECTOR('',#25901,0.999999999999999);
#3622=VECTOR('',#25902,1.);
#3623=VECTOR('',#25903,0.999999999999999);
#3624=VECTOR('',#25908,1.);
#3625=VECTOR('',#25911,1.);
#3626=VECTOR('',#25916,1.);
#3627=VECTOR('',#25923,1.);
#3628=VECTOR('',#25928,1.);
#3629=VECTOR('',#25929,1.);
#3630=VECTOR('',#25930,1.);
#3631=VECTOR('',#25935,1.);
#3632=VECTOR('',#25938,1.);
#3633=VECTOR('',#25943,1.);
#3634=VECTOR('',#25950,1.);
#3635=VECTOR('',#25955,1.);
#3636=VECTOR('',#25956,1.);
#3637=VECTOR('',#25957,1.);
#3638=VECTOR('',#25960,1.);
#3639=VECTOR('',#25961,1.);
#3640=VECTOR('',#25962,1.);
#3641=VECTOR('',#25965,0.999999999999999);
#3642=VECTOR('',#25966,1.);
#3643=VECTOR('',#25967,0.999999999999999);
#3644=VECTOR('',#25970,1.);
#3645=VECTOR('',#25971,1.);
#3646=VECTOR('',#25972,1.);
#3647=VECTOR('',#25975,1.);
#3648=VECTOR('',#25976,1.);
#3649=VECTOR('',#25977,1.);
#3650=VECTOR('',#25982,1.);
#3651=VECTOR('',#25993,1.);
#3652=VECTOR('',#25996,1.);
#3653=VECTOR('',#26003,1.);
#3654=VECTOR('',#26010,1.);
#3655=VECTOR('',#26013,1.);
#3656=VECTOR('',#26018,1.);
#3657=VECTOR('',#26025,1.);
#3658=VECTOR('',#26028,1.);
#3659=VECTOR('',#26031,1.);
#3660=VECTOR('',#26038,1.);
#3661=VECTOR('',#26051,0.0025);
#3662=VECTOR('',#26058,0.003875);
#3663=VECTOR('',#26065,1.);
#3664=VECTOR('',#26066,1.);
#3665=VECTOR('',#26067,1.);
#3666=VECTOR('',#26068,1.);
#3667=VECTOR('',#26071,1.);
#3668=VECTOR('',#26072,1.);
#3669=VECTOR('',#26073,1.);
#3670=VECTOR('',#26076,1.);
#3671=VECTOR('',#26079,1.);
#3672=VECTOR('',#26080,1.);
#3673=VECTOR('',#26081,1.);
#3674=VECTOR('',#26084,1.);
#3675=VECTOR('',#26085,1.);
#3676=VECTOR('',#26090,1.);
#3677=VECTOR('',#26091,1.);
#3678=VECTOR('',#26092,1.);
#3679=VECTOR('',#26093,1.);
#3680=VECTOR('',#26098,1.);
#3681=VECTOR('',#26101,1.);
#3682=VECTOR('',#26108,1.);
#3683=VECTOR('',#26111,1.);
#3684=VECTOR('',#26116,1.);
#3685=VECTOR('',#26119,1.);
#3686=VECTOR('',#26124,1.);
#3687=VECTOR('',#26127,1.);
#3688=VECTOR('',#26132,1.);
#3689=VECTOR('',#26135,1.);
#3690=VECTOR('',#26140,1.);
#3691=VECTOR('',#26143,1.);
#3692=VECTOR('',#26148,1.);
#3693=VECTOR('',#26151,1.);
#3694=VECTOR('',#26156,1.);
#3695=VECTOR('',#26159,1.);
#3696=VECTOR('',#26164,1.);
#3697=VECTOR('',#26167,1.);
#3698=VECTOR('',#26172,1.);
#3699=VECTOR('',#26175,1.);
#3700=VECTOR('',#26180,1.);
#3701=VECTOR('',#26183,1.);
#3702=VECTOR('',#26188,1.);
#3703=VECTOR('',#26191,1.);
#3704=VECTOR('',#26196,1.);
#3705=VECTOR('',#26199,1.);
#3706=VECTOR('',#26204,1.);
#3707=VECTOR('',#26207,1.);
#3708=VECTOR('',#26212,1.);
#3709=VECTOR('',#26215,1.);
#3710=VECTOR('',#26220,1.);
#3711=VECTOR('',#26223,1.);
#3712=VECTOR('',#26228,1.);
#3713=VECTOR('',#26231,1.);
#3714=VECTOR('',#26236,1.);
#3715=VECTOR('',#26239,1.);
#3716=VECTOR('',#26244,1.);
#3717=VECTOR('',#26247,1.);
#3718=VECTOR('',#26252,1.);
#3719=VECTOR('',#26255,1.);
#3720=VECTOR('',#26260,1.);
#3721=VECTOR('',#26263,1.);
#3722=VECTOR('',#26268,1.);
#3723=VECTOR('',#26271,1.);
#3724=VECTOR('',#26276,1.);
#3725=VECTOR('',#26279,1.);
#3726=VECTOR('',#26284,1.);
#3727=VECTOR('',#26287,1.);
#3728=VECTOR('',#26292,1.);
#3729=VECTOR('',#26295,1.);
#3730=VECTOR('',#26300,1.);
#3731=VECTOR('',#26303,1.);
#3732=VECTOR('',#26308,1.);
#3733=VECTOR('',#26311,1.);
#3734=VECTOR('',#26316,1.);
#3735=VECTOR('',#26319,1.);
#3736=VECTOR('',#26324,1.);
#3737=VECTOR('',#26327,1.);
#3738=VECTOR('',#26332,1.);
#3739=VECTOR('',#26335,1.);
#3740=VECTOR('',#26340,1.);
#3741=VECTOR('',#26343,1.);
#3742=VECTOR('',#26348,1.);
#3743=VECTOR('',#26351,1.);
#3744=VECTOR('',#26356,1.);
#3745=VECTOR('',#26359,1.);
#3746=VECTOR('',#26364,1.);
#3747=VECTOR('',#26367,1.);
#3748=VECTOR('',#26372,1.);
#3749=VECTOR('',#26375,1.);
#3750=VECTOR('',#26380,1.);
#3751=VECTOR('',#26383,1.);
#3752=VECTOR('',#26388,1.);
#3753=VECTOR('',#26391,1.);
#3754=VECTOR('',#26396,1.);
#3755=VECTOR('',#26399,1.);
#3756=VECTOR('',#26404,1.);
#3757=VECTOR('',#26407,1.);
#3758=VECTOR('',#26412,1.);
#3759=VECTOR('',#26415,1.);
#3760=VECTOR('',#26420,1.);
#3761=VECTOR('',#26423,1.);
#3762=VECTOR('',#26428,1.);
#3763=VECTOR('',#26431,1.);
#3764=VECTOR('',#26436,1.);
#3765=VECTOR('',#26439,1.);
#3766=VECTOR('',#26444,1.);
#3767=VECTOR('',#26447,1.);
#3768=VECTOR('',#26452,1.);
#3769=VECTOR('',#26455,1.);
#3770=VECTOR('',#26558,1.);
#3771=VECTOR('',#26561,1.);
#3772=VECTOR('',#26746,0.0025);
#3773=VECTOR('',#26763,0.0025);
#3774=VECTOR('',#26782,0.00433333333333334);
#3775=VECTOR('',#26789,1.);
#3776=VECTOR('',#26792,1.);
#3777=VECTOR('',#26797,1.);
#3778=VECTOR('',#26804,1.);
#3779=VECTOR('',#26809,1.);
#3780=VECTOR('',#26810,1.);
#3781=VECTOR('',#26811,1.);
#3782=VECTOR('',#26816,1.);
#3783=VECTOR('',#26819,1.);
#3784=VECTOR('',#26824,1.);
#3785=VECTOR('',#26831,1.);
#3786=VECTOR('',#26836,1.);
#3787=VECTOR('',#26837,1.);
#3788=VECTOR('',#26838,1.);
#3789=VECTOR('',#26843,1.);
#3790=VECTOR('',#26846,1.);
#3791=VECTOR('',#26851,1.);
#3792=VECTOR('',#26858,1.);
#3793=VECTOR('',#26863,1.);
#3794=VECTOR('',#26864,1.);
#3795=VECTOR('',#26865,1.);
#3796=VECTOR('',#26870,1.);
#3797=VECTOR('',#26873,1.);
#3798=VECTOR('',#26878,1.);
#3799=VECTOR('',#26885,1.);
#3800=VECTOR('',#26890,1.);
#3801=VECTOR('',#26891,1.);
#3802=VECTOR('',#26892,1.);
#3803=VECTOR('',#26897,1.);
#3804=VECTOR('',#26900,1.);
#3805=VECTOR('',#26905,1.);
#3806=VECTOR('',#26912,1.);
#3807=VECTOR('',#26917,1.);
#3808=VECTOR('',#26918,1.);
#3809=VECTOR('',#26919,1.);
#3810=VECTOR('',#26922,1.);
#3811=VECTOR('',#26923,1.);
#3812=VECTOR('',#26924,1.);
#3813=VECTOR('',#26927,1.);
#3814=VECTOR('',#26928,1.);
#3815=VECTOR('',#26929,1.);
#3816=VECTOR('',#26932,1.);
#3817=VECTOR('',#26933,1.);
#3818=VECTOR('',#26934,1.);
#3819=VECTOR('',#26937,1.);
#3820=VECTOR('',#26938,1.);
#3821=VECTOR('',#26939,1.);
#3822=VECTOR('',#26944,1.);
#3823=VECTOR('',#26955,1.);
#3824=VECTOR('',#26958,1.);
#3825=VECTOR('',#26965,1.);
#3826=VECTOR('',#26972,1.);
#3827=VECTOR('',#26975,1.);
#3828=VECTOR('',#26980,1.);
#3829=VECTOR('',#26987,1.);
#3830=VECTOR('',#26988,1.);
#3831=VECTOR('',#26993,1.);
#3832=VECTOR('',#26996,1.);
#3833=VECTOR('',#27007,1.);
#3834=VECTOR('',#27008,1.);
#3835=VECTOR('',#27009,1.);
#3836=VECTOR('',#27010,1.);
#3837=VECTOR('',#27013,1.);
#3838=VECTOR('',#27014,1.);
#3839=VECTOR('',#27015,1.);
#3840=VECTOR('',#27016,1.);
#3841=VECTOR('',#27019,1.);
#3842=VECTOR('',#27020,1.);
#3843=VECTOR('',#27025,1.);
#3844=VECTOR('',#27026,1.);
#3845=VECTOR('',#27027,1.);
#3846=VECTOR('',#27030,1.);
#3847=VECTOR('',#27035,1.);
#3848=VECTOR('',#27036,1.);
#3849=VECTOR('',#27037,1.);
#3850=VECTOR('',#27040,1.);
#3851=VECTOR('',#27043,1.);
#3852=VECTOR('',#27050,0.01);
#3853=VECTOR('',#27053,0.01);
#3854=VECTOR('',#27058,0.01);
#3855=VECTOR('',#27059,1.);
#3856=VECTOR('',#27060,1.);
#3857=VECTOR('',#27063,0.01);
#3858=VECTOR('',#27070,0.01);
#3859=VECTOR('',#27077,0.01);
#3860=VECTOR('',#27084,0.01);
#3861=VECTOR('',#27085,1.);
#3862=VECTOR('',#27086,1.);
#3863=VECTOR('',#27089,1.);
#3864=VECTOR('',#27096,1.);
#3865=VECTOR('',#27103,0.01);
#3866=VECTOR('',#27106,0.01);
#3867=VECTOR('',#27111,1.);
#3868=VECTOR('',#27112,0.01);
#3869=VECTOR('',#27113,1.);
#3870=VECTOR('',#27118,0.01);
#3871=VECTOR('',#27125,0.01);
#3872=VECTOR('',#27132,0.01);
#3873=VECTOR('',#27137,1.);
#3874=VECTOR('',#27138,0.01);
#3875=VECTOR('',#27139,1.);
#3876=VECTOR('',#27158,1.);
#3877=VECTOR('',#27159,1.);
#3878=VECTOR('',#27160,1.);
#3879=VECTOR('',#27161,1.);
#3880=VECTOR('',#27162,1.);
#3881=VECTOR('',#27163,1.);
#3882=VECTOR('',#27164,1.);
#3883=VECTOR('',#27165,1.);
#3884=VECTOR('',#27172,0.0017);
#3885=VECTOR('',#27177,0.0017);
#3886=VECTOR('',#27182,0.0017);
#3887=VECTOR('',#27187,0.0017);
#3888=VECTOR('',#27192,1.);
#3889=VECTOR('',#27193,1.);
#3890=VECTOR('',#27194,1.);
#3891=VECTOR('',#27197,1.);
#3892=VECTOR('',#27198,1.);
#3893=VECTOR('',#27201,1.);
#3894=VECTOR('',#27202,1.);
#3895=VECTOR('',#27205,1.);
#3896=VECTOR('',#27206,1.);
#3897=VECTOR('',#27209,1.);
#3898=VECTOR('',#27210,1.);
#3899=VECTOR('',#27213,1.);
#3900=VECTOR('',#27214,1.);
#3901=VECTOR('',#27217,1.);
#3902=VECTOR('',#27218,1.);
#3903=VECTOR('',#27221,1.);
#3904=VECTOR('',#27230,1.);
#3905=VECTOR('',#27233,1.);
#3906=VECTOR('',#27238,1.);
#3907=VECTOR('',#27245,1.);
#3908=VECTOR('',#27250,1.);
#3909=VECTOR('',#27251,1.);
#3910=VECTOR('',#27252,1.);
#3911=VECTOR('',#27257,1.);
#3912=VECTOR('',#27260,1.);
#3913=VECTOR('',#27265,1.);
#3914=VECTOR('',#27272,1.);
#3915=VECTOR('',#27277,1.);
#3916=VECTOR('',#27278,1.);
#3917=VECTOR('',#27279,1.);
#3918=VECTOR('',#27284,1.);
#3919=VECTOR('',#27287,1.);
#3920=VECTOR('',#27292,1.);
#3921=VECTOR('',#27299,1.);
#3922=VECTOR('',#27304,1.);
#3923=VECTOR('',#27305,1.);
#3924=VECTOR('',#27306,1.);
#3925=VECTOR('',#27311,1.);
#3926=VECTOR('',#27314,1.);
#3927=VECTOR('',#27319,1.);
#3928=VECTOR('',#27326,1.);
#3929=VECTOR('',#27331,1.);
#3930=VECTOR('',#27332,1.);
#3931=VECTOR('',#27333,1.);
#3932=VECTOR('',#27338,1.);
#3933=VECTOR('',#27341,1.);
#3934=VECTOR('',#27346,1.);
#3935=VECTOR('',#27353,1.);
#3936=VECTOR('',#27358,1.);
#3937=VECTOR('',#27359,1.);
#3938=VECTOR('',#27360,1.);
#3939=VECTOR('',#27363,1.);
#3940=VECTOR('',#27364,1.);
#3941=VECTOR('',#27365,1.);
#3942=VECTOR('',#27368,1.);
#3943=VECTOR('',#27369,1.);
#3944=VECTOR('',#27370,1.);
#3945=VECTOR('',#27373,1.);
#3946=VECTOR('',#27374,1.);
#3947=VECTOR('',#27375,1.);
#3948=VECTOR('',#27378,1.);
#3949=VECTOR('',#27379,1.);
#3950=VECTOR('',#27380,1.);
#3951=VECTOR('',#27385,1.);
#3952=VECTOR('',#27396,0.999999999999999);
#3953=VECTOR('',#27399,0.999999999999999);
#3954=VECTOR('',#27406,1.);
#3955=VECTOR('',#27413,1.);
#3956=VECTOR('',#27416,1.);
#3957=VECTOR('',#27421,1.);
#3958=VECTOR('',#27428,1.);
#3959=VECTOR('',#27431,1.);
#3960=VECTOR('',#27434,0.999999999999999);
#3961=VECTOR('',#27441,0.999999999999999);
#3962=VECTOR('',#27448,1.);
#3963=VECTOR('',#27449,1.);
#3964=VECTOR('',#27450,1.);
#3965=VECTOR('',#27451,1.);
#3966=VECTOR('',#27454,1.);
#3967=VECTOR('',#27455,1.);
#3968=VECTOR('',#27456,1.);
#3969=VECTOR('',#27459,1.);
#3970=VECTOR('',#27460,1.);
#3971=VECTOR('',#27461,1.);
#3972=VECTOR('',#27464,1.);
#3973=VECTOR('',#27465,1.);
#3974=VECTOR('',#27468,1.);
#3975=VECTOR('',#27469,1.);
#3976=VECTOR('',#27470,1.);
#3977=VECTOR('',#27471,1.);
#3978=VECTOR('',#27474,1.);
#3979=VECTOR('',#27475,1.);
#3980=VECTOR('',#27476,1.);
#3981=VECTOR('',#27479,1.);
#3982=VECTOR('',#27480,1.);
#3983=VECTOR('',#27481,1.);
#3984=VECTOR('',#27484,1.);
#3985=VECTOR('',#27485,1.);
#3986=VECTOR('',#27488,1.);
#3987=VECTOR('',#27489,1.);
#3988=VECTOR('',#27490,1.);
#3989=VECTOR('',#27491,1.);
#3990=VECTOR('',#27494,1.);
#3991=VECTOR('',#27495,1.);
#3992=VECTOR('',#27496,1.);
#3993=VECTOR('',#27499,1.);
#3994=VECTOR('',#27500,1.);
#3995=VECTOR('',#27501,1.);
#3996=VECTOR('',#27504,1.);
#3997=VECTOR('',#27505,1.);
#3998=VECTOR('',#27508,1.);
#3999=VECTOR('',#27509,1.);
#4000=VECTOR('',#27510,1.);
#4001=VECTOR('',#27511,1.);
#4002=VECTOR('',#27514,1.);
#4003=VECTOR('',#27515,1.);
#4004=VECTOR('',#27516,1.);
#4005=VECTOR('',#27519,1.);
#4006=VECTOR('',#27520,1.);
#4007=VECTOR('',#27521,1.);
#4008=VECTOR('',#27524,1.);
#4009=VECTOR('',#27525,1.);
#4010=VECTOR('',#27528,1.);
#4011=VECTOR('',#27529,1.);
#4012=VECTOR('',#27530,1.);
#4013=VECTOR('',#27531,1.);
#4014=VECTOR('',#27534,1.);
#4015=VECTOR('',#27535,1.);
#4016=VECTOR('',#27536,1.);
#4017=VECTOR('',#27539,1.);
#4018=VECTOR('',#27540,1.);
#4019=VECTOR('',#27541,1.);
#4020=VECTOR('',#27544,1.);
#4021=VECTOR('',#27545,1.);
#4022=VECTOR('',#27548,1.);
#4023=VECTOR('',#27549,1.);
#4024=VECTOR('',#27550,1.);
#4025=VECTOR('',#27551,1.);
#4026=VECTOR('',#27554,1.);
#4027=VECTOR('',#27555,1.);
#4028=VECTOR('',#27556,1.);
#4029=VECTOR('',#27559,1.);
#4030=VECTOR('',#27560,1.);
#4031=VECTOR('',#27561,1.);
#4032=VECTOR('',#27564,1.);
#4033=VECTOR('',#27565,1.);
#4034=VECTOR('',#27568,1.);
#4035=VECTOR('',#27569,1.);
#4036=VECTOR('',#27570,1.);
#4037=VECTOR('',#27571,1.);
#4038=VECTOR('',#27574,1.);
#4039=VECTOR('',#27575,1.);
#4040=VECTOR('',#27576,1.);
#4041=VECTOR('',#27579,1.);
#4042=VECTOR('',#27580,1.);
#4043=VECTOR('',#27581,1.);
#4044=VECTOR('',#27584,1.);
#4045=VECTOR('',#27585,1.);
#4046=VECTOR('',#27586,1.);
#4047=VECTOR('',#27587,1.);
#4048=VECTOR('',#27588,1.);
#4049=VECTOR('',#27591,1.);
#4050=VECTOR('',#27592,1.);
#4051=VECTOR('',#27593,1.);
#4052=VECTOR('',#27594,1.);
#4053=VECTOR('',#27597,1.);
#4054=VECTOR('',#27598,1.);
#4055=VECTOR('',#27599,1.);
#4056=VECTOR('',#27602,1.);
#4057=VECTOR('',#27603,1.);
#4058=VECTOR('',#27604,1.);
#4059=VECTOR('',#27605,1.);
#4060=VECTOR('',#27606,1.);
#4061=VECTOR('',#27607,1.);
#4062=VECTOR('',#27608,1.);
#4063=VECTOR('',#27609,1.);
#4064=VECTOR('',#27610,1.);
#4065=VECTOR('',#27611,1.);
#4066=VECTOR('',#27614,1.);
#4067=VECTOR('',#27615,1.);
#4068=VECTOR('',#27616,1.);
#4069=VECTOR('',#27619,1.);
#4070=VECTOR('',#27620,1.);
#4071=VECTOR('',#27621,1.);
#4072=VECTOR('',#27622,1.);
#4073=VECTOR('',#27625,1.);
#4074=VECTOR('',#27626,1.);
#4075=VECTOR('',#27629,1.);
#4076=VECTOR('',#27630,1.);
#4077=VECTOR('',#27631,1.);
#4078=VECTOR('',#27632,1.);
#4079=VECTOR('',#27635,1.);
#4080=VECTOR('',#27636,1.);
#4081=VECTOR('',#27637,1.);
#4082=VECTOR('',#27638,1.);
#4083=VECTOR('',#27639,1.);
#4084=VECTOR('',#27640,1.);
#4085=VECTOR('',#27641,1.);
#4086=VECTOR('',#27642,1.);
#4087=VECTOR('',#27643,1.);
#4088=VECTOR('',#27646,1.);
#4089=VECTOR('',#27647,1.);
#4090=VECTOR('',#27648,1.);
#4091=VECTOR('',#27651,1.);
#4092=VECTOR('',#27652,1.);
#4093=VECTOR('',#27653,1.);
#4094=VECTOR('',#27656,1.);
#4095=VECTOR('',#27659,1.);
#4096=VECTOR('',#27660,1.);
#4097=VECTOR('',#27661,1.);
#4098=VECTOR('',#27662,1.);
#4099=VECTOR('',#27665,1.);
#4100=VECTOR('',#27666,1.);
#4101=VECTOR('',#27667,1.);
#4102=VECTOR('',#27670,1.);
#4103=VECTOR('',#27671,1.);
#4104=VECTOR('',#27672,1.);
#4105=VECTOR('',#27675,1.);
#4106=VECTOR('',#27676,1.);
#4107=VECTOR('',#27677,1.);
#4108=VECTOR('',#27678,1.);
#4109=VECTOR('',#27681,1.);
#4110=VECTOR('',#27682,1.);
#4111=VECTOR('',#27683,1.);
#4112=VECTOR('',#27688,1.);
#4113=VECTOR('',#27691,1.);
#4114=VECTOR('',#27692,1.);
#4115=VECTOR('',#27693,1.);
#4116=VECTOR('',#27694,1.);
#4117=VECTOR('',#27697,1.);
#4118=VECTOR('',#27698,1.);
#4119=VECTOR('',#27701,1.);
#4120=VECTOR('',#27702,1.);
#4121=VECTOR('',#27703,1.);
#4122=VECTOR('',#27704,1.);
#4123=VECTOR('',#27707,1.);
#4124=VECTOR('',#27708,1.);
#4125=VECTOR('',#27711,1.);
#4126=VECTOR('',#27714,1.);
#4127=VECTOR('',#27717,1.);
#4128=VECTOR('',#27726,0.0025);
#4129=VECTOR('',#27733,0.012);
#4130=VECTOR('',#27746,1.);
#4131=VECTOR('',#27749,1.);
#4132=VECTOR('',#27754,1.);
#4133=VECTOR('',#27761,1.);
#4134=VECTOR('',#27766,1.);
#4135=VECTOR('',#27767,1.);
#4136=VECTOR('',#27768,1.);
#4137=VECTOR('',#27773,1.);
#4138=VECTOR('',#27776,1.);
#4139=VECTOR('',#27781,1.);
#4140=VECTOR('',#27788,1.);
#4141=VECTOR('',#27793,0.999999999999999);
#4142=VECTOR('',#27794,1.);
#4143=VECTOR('',#27795,0.999999999999999);
#4144=VECTOR('',#27800,1.);
#4145=VECTOR('',#27803,1.);
#4146=VECTOR('',#27808,1.);
#4147=VECTOR('',#27815,1.);
#4148=VECTOR('',#27820,1.);
#4149=VECTOR('',#27821,1.);
#4150=VECTOR('',#27822,1.);
#4151=VECTOR('',#27827,1.);
#4152=VECTOR('',#27830,1.);
#4153=VECTOR('',#27835,1.);
#4154=VECTOR('',#27842,1.);
#4155=VECTOR('',#27847,1.);
#4156=VECTOR('',#27848,1.);
#4157=VECTOR('',#27849,1.);
#4158=VECTOR('',#27854,1.);
#4159=VECTOR('',#27857,1.);
#4160=VECTOR('',#27862,1.);
#4161=VECTOR('',#27869,1.);
#4162=VECTOR('',#27874,1.);
#4163=VECTOR('',#27875,1.);
#4164=VECTOR('',#27876,1.);
#4165=VECTOR('',#27879,1.);
#4166=VECTOR('',#27880,1.);
#4167=VECTOR('',#27881,1.);
#4168=VECTOR('',#27884,0.999999999999999);
#4169=VECTOR('',#27885,1.);
#4170=VECTOR('',#27886,0.999999999999999);
#4171=VECTOR('',#27889,1.);
#4172=VECTOR('',#27890,1.);
#4173=VECTOR('',#27891,1.);
#4174=VECTOR('',#27894,1.);
#4175=VECTOR('',#27895,1.);
#4176=VECTOR('',#27896,1.);
#4177=VECTOR('',#27901,1.);
#4178=VECTOR('',#27912,1.);
#4179=VECTOR('',#27915,1.);
#4180=VECTOR('',#27922,1.);
#4181=VECTOR('',#27929,1.);
#4182=VECTOR('',#27932,1.);
#4183=VECTOR('',#27937,1.);
#4184=VECTOR('',#27944,1.);
#4185=VECTOR('',#27945,1.);
#4186=VECTOR('',#27950,1.);
#4187=VECTOR('',#27953,1.);
#4188=VECTOR('',#27966,1.);
#4189=VECTOR('',#27969,1.);
#4190=VECTOR('',#27974,1.);
#4191=VECTOR('',#27981,1.);
#4192=VECTOR('',#27986,1.);
#4193=VECTOR('',#27987,1.);
#4194=VECTOR('',#27988,1.);
#4195=VECTOR('',#27993,1.);
#4196=VECTOR('',#27996,1.);
#4197=VECTOR('',#28001,1.);
#4198=VECTOR('',#28008,1.);
#4199=VECTOR('',#28013,0.999999999999999);
#4200=VECTOR('',#28014,1.);
#4201=VECTOR('',#28015,0.999999999999999);
#4202=VECTOR('',#28020,1.);
#4203=VECTOR('',#28023,1.);
#4204=VECTOR('',#28028,1.);
#4205=VECTOR('',#28035,1.);
#4206=VECTOR('',#28040,1.);
#4207=VECTOR('',#28041,1.);
#4208=VECTOR('',#28042,1.);
#4209=VECTOR('',#28047,1.);
#4210=VECTOR('',#28050,1.);
#4211=VECTOR('',#28055,1.);
#4212=VECTOR('',#28062,1.);
#4213=VECTOR('',#28067,1.);
#4214=VECTOR('',#28068,1.);
#4215=VECTOR('',#28069,1.);
#4216=VECTOR('',#28074,1.);
#4217=VECTOR('',#28077,1.);
#4218=VECTOR('',#28082,1.);
#4219=VECTOR('',#28089,1.);
#4220=VECTOR('',#28094,1.);
#4221=VECTOR('',#28095,1.);
#4222=VECTOR('',#28096,1.);
#4223=VECTOR('',#28099,1.);
#4224=VECTOR('',#28100,1.);
#4225=VECTOR('',#28101,1.);
#4226=VECTOR('',#28104,0.999999999999999);
#4227=VECTOR('',#28105,1.);
#4228=VECTOR('',#28106,0.999999999999999);
#4229=VECTOR('',#28109,1.);
#4230=VECTOR('',#28110,1.);
#4231=VECTOR('',#28111,1.);
#4232=VECTOR('',#28114,1.);
#4233=VECTOR('',#28115,1.);
#4234=VECTOR('',#28116,1.);
#4235=VECTOR('',#28121,1.);
#4236=VECTOR('',#28132,1.);
#4237=VECTOR('',#28135,1.);
#4238=VECTOR('',#28142,1.);
#4239=VECTOR('',#28149,1.);
#4240=VECTOR('',#28152,1.);
#4241=VECTOR('',#28157,1.);
#4242=VECTOR('',#28164,1.);
#4243=VECTOR('',#28165,1.);
#4244=VECTOR('',#28170,1.);
#4245=VECTOR('',#28173,1.);
#4246=VECTOR('',#28196,0.0025);
#4247=VECTOR('',#28215,0.00433333333333334);
#4248=VECTOR('',#28220,1.);
#4249=VECTOR('',#28221,1.);
#4250=VECTOR('',#28222,1.);
#4251=VECTOR('',#28223,1.);
#4252=VECTOR('',#28226,1.);
#4253=VECTOR('',#28227,1.);
#4254=VECTOR('',#28228,1.);
#4255=VECTOR('',#28229,1.);
#4256=VECTOR('',#28232,1.);
#4257=VECTOR('',#28239,1.);
#4258=VECTOR('',#28240,1.);
#4259=VECTOR('',#28243,1.);
#4260=VECTOR('',#28244,1.);
#4261=VECTOR('',#28245,1.);
#4262=VECTOR('',#28248,1.);
#4263=VECTOR('',#28249,1.);
#4264=VECTOR('',#28252,1.);
#4265=VECTOR('',#28253,1.);
#4266=VECTOR('',#28256,1.);
#4267=VECTOR('',#28265,0.0013466375);
#4268=VECTOR('',#28272,0.0015);
#4269=VECTOR('',#28351,0.00277242641351798);
#4270=VECTOR('',#28354,1.);
#4271=VECTOR('',#28355,1.);
#4272=VECTOR('',#28360,1.);
#4273=VECTOR('',#28363,1.);
#4274=VECTOR('',#28366,1.);
#4275=VECTOR('',#28373,1.);
#4276=VECTOR('',#28376,1.);
#4277=VECTOR('',#28381,1.);
#4278=VECTOR('',#28386,0.000409956151237738);
#4279=VECTOR('',#28391,0.001364685);
#4280=VECTOR('',#28398,0.0014323425);
#4281=CYLINDRICAL_SURFACE('',#19958,0.008);
#4282=CYLINDRICAL_SURFACE('',#19968,0.00616666666666666);
#4283=CYLINDRICAL_SURFACE('',#19970,0.00025);
#4284=CYLINDRICAL_SURFACE('',#19973,0.01345);
#4285=CYLINDRICAL_SURFACE('',#19976,0.00025);
#4286=CYLINDRICAL_SURFACE('',#19980,0.00025);
#4287=CYLINDRICAL_SURFACE('',#19983,0.01345);
#4288=CYLINDRICAL_SURFACE('',#19986,0.00025);
#4289=CYLINDRICAL_SURFACE('',#19990,0.00025);
#4290=CYLINDRICAL_SURFACE('',#19993,0.01345);
#4291=CYLINDRICAL_SURFACE('',#19996,0.00025);
#4292=CYLINDRICAL_SURFACE('',#20000,0.00025);
#4293=CYLINDRICAL_SURFACE('',#20003,0.01345);
#4294=CYLINDRICAL_SURFACE('',#20006,0.00025);
#4295=CYLINDRICAL_SURFACE('',#20010,0.00025);
#4296=CYLINDRICAL_SURFACE('',#20013,0.01345);
#4297=CYLINDRICAL_SURFACE('',#20016,0.00025);
#4298=CYLINDRICAL_SURFACE('',#20024,0.013);
#4299=CYLINDRICAL_SURFACE('',#20027,0.013);
#4300=CYLINDRICAL_SURFACE('',#20036,0.013);
#4301=CYLINDRICAL_SURFACE('',#20038,0.013);
#4302=CYLINDRICAL_SURFACE('',#20041,0.013);
#4303=CYLINDRICAL_SURFACE('',#20043,0.0139);
#4304=CYLINDRICAL_SURFACE('',#20046,0.013);
#4305=CYLINDRICAL_SURFACE('',#20054,0.0025);
#4306=CYLINDRICAL_SURFACE('',#20056,0.0045);
#4307=CYLINDRICAL_SURFACE('',#20060,0.01465);
#4308=CYLINDRICAL_SURFACE('',#20077,0.0139);
#4309=CYLINDRICAL_SURFACE('',#20083,0.0015);
#4310=CYLINDRICAL_SURFACE('',#20085,0.0015);
#4311=CYLINDRICAL_SURFACE('',#20088,0.01465);
#4312=CYLINDRICAL_SURFACE('',#20105,0.0139);
#4313=CYLINDRICAL_SURFACE('',#20111,0.0015);
#4314=CYLINDRICAL_SURFACE('',#20113,0.0015);
#4315=CYLINDRICAL_SURFACE('',#20116,0.01465);
#4316=CYLINDRICAL_SURFACE('',#20133,0.0139);
#4317=CYLINDRICAL_SURFACE('',#20139,0.0015);
#4318=CYLINDRICAL_SURFACE('',#20141,0.0015);
#4319=CYLINDRICAL_SURFACE('',#20144,0.01465);
#4320=CYLINDRICAL_SURFACE('',#20161,0.0139);
#4321=CYLINDRICAL_SURFACE('',#20167,0.0015);
#4322=CYLINDRICAL_SURFACE('',#20169,0.0015);
#4323=CYLINDRICAL_SURFACE('',#20172,0.01465);
#4324=CYLINDRICAL_SURFACE('',#20189,0.0139);
#4325=CYLINDRICAL_SURFACE('',#20195,0.0015);
#4326=CYLINDRICAL_SURFACE('',#20197,0.0015);
#4327=CYLINDRICAL_SURFACE('',#20200,0.01465);
#4328=CYLINDRICAL_SURFACE('',#20217,0.0139);
#4329=CYLINDRICAL_SURFACE('',#20223,0.0015);
#4330=CYLINDRICAL_SURFACE('',#20225,0.0015);
#4331=CYLINDRICAL_SURFACE('',#20228,0.01465);
#4332=CYLINDRICAL_SURFACE('',#20245,0.0139);
#4333=CYLINDRICAL_SURFACE('',#20251,0.0015);
#4334=CYLINDRICAL_SURFACE('',#20253,0.0015);
#4335=CYLINDRICAL_SURFACE('',#20256,0.01465);
#4336=CYLINDRICAL_SURFACE('',#20273,0.0139);
#4337=CYLINDRICAL_SURFACE('',#20279,0.0015);
#4338=CYLINDRICAL_SURFACE('',#20281,0.0015);
#4339=CYLINDRICAL_SURFACE('',#20316,0.0005);
#4340=CYLINDRICAL_SURFACE('',#20319,0.0005);
#4341=CYLINDRICAL_SURFACE('',#20322,0.0005);
#4342=CYLINDRICAL_SURFACE('',#20325,0.0005);
#4343=CYLINDRICAL_SURFACE('',#20328,0.0005);
#4344=CYLINDRICAL_SURFACE('',#20331,0.0005);
#4345=CYLINDRICAL_SURFACE('',#20334,0.0005);
#4346=CYLINDRICAL_SURFACE('',#20337,0.0005);
#4347=CYLINDRICAL_SURFACE('',#20340,0.0005);
#4348=CYLINDRICAL_SURFACE('',#20343,0.0005);
#4349=CYLINDRICAL_SURFACE('',#20346,0.0005);
#4350=CYLINDRICAL_SURFACE('',#20349,0.0005);
#4351=CYLINDRICAL_SURFACE('',#20352,0.0005);
#4352=CYLINDRICAL_SURFACE('',#20355,0.0005);
#4353=CYLINDRICAL_SURFACE('',#20358,0.0005);
#4354=CYLINDRICAL_SURFACE('',#20361,0.0005);
#4355=CYLINDRICAL_SURFACE('',#20364,0.0005);
#4356=CYLINDRICAL_SURFACE('',#20367,0.0005);
#4357=CYLINDRICAL_SURFACE('',#20370,0.0005);
#4358=CYLINDRICAL_SURFACE('',#20373,0.0005);
#4359=CYLINDRICAL_SURFACE('',#20376,0.0005);
#4360=CYLINDRICAL_SURFACE('',#20379,0.0005);
#4361=CYLINDRICAL_SURFACE('',#20382,0.0005);
#4362=CYLINDRICAL_SURFACE('',#20385,0.0005);
#4363=CYLINDRICAL_SURFACE('',#20388,0.0005);
#4364=CYLINDRICAL_SURFACE('',#20391,0.0005);
#4365=CYLINDRICAL_SURFACE('',#20394,0.0005);
#4366=CYLINDRICAL_SURFACE('',#20397,0.0005);
#4367=CYLINDRICAL_SURFACE('',#20400,0.0005);
#4368=CYLINDRICAL_SURFACE('',#20403,0.0005);
#4369=CYLINDRICAL_SURFACE('',#20406,0.0005);
#4370=CYLINDRICAL_SURFACE('',#20409,0.0005);
#4371=CYLINDRICAL_SURFACE('',#20412,0.0005);
#4372=CYLINDRICAL_SURFACE('',#20415,0.0005);
#4373=CYLINDRICAL_SURFACE('',#20418,0.0005);
#4374=CYLINDRICAL_SURFACE('',#20421,0.0005);
#4375=CYLINDRICAL_SURFACE('',#20424,0.0005);
#4376=CYLINDRICAL_SURFACE('',#20427,0.0005);
#4377=CYLINDRICAL_SURFACE('',#20430,0.0005);
#4378=CYLINDRICAL_SURFACE('',#20433,0.0005);
#4379=CYLINDRICAL_SURFACE('',#20436,0.0005);
#4380=CYLINDRICAL_SURFACE('',#20439,0.0005);
#4381=CYLINDRICAL_SURFACE('',#20442,0.0005);
#4382=CYLINDRICAL_SURFACE('',#20445,0.0005);
#4383=CYLINDRICAL_SURFACE('',#20496,0.0129);
#4384=CYLINDRICAL_SURFACE('',#20498,0.0129);
#4385=CYLINDRICAL_SURFACE('',#20500,0.0129);
#4386=CYLINDRICAL_SURFACE('',#20502,0.0129);
#4387=CYLINDRICAL_SURFACE('',#20504,0.0129);
#4388=CYLINDRICAL_SURFACE('',#20506,0.0129);
#4389=CYLINDRICAL_SURFACE('',#20508,0.0129);
#4390=CYLINDRICAL_SURFACE('',#20510,0.0129);
#4391=CYLINDRICAL_SURFACE('',#20512,0.0129);
#4392=CYLINDRICAL_SURFACE('',#20514,0.0129);
#4393=CYLINDRICAL_SURFACE('',#20516,0.0129);
#4394=CYLINDRICAL_SURFACE('',#20518,0.0129);
#4395=CYLINDRICAL_SURFACE('',#20520,0.0129);
#4396=CYLINDRICAL_SURFACE('',#20522,0.0129);
#4397=CYLINDRICAL_SURFACE('',#20524,0.0129);
#4398=CYLINDRICAL_SURFACE('',#20526,0.0129);
#4399=CYLINDRICAL_SURFACE('',#20528,0.0129);
#4400=CYLINDRICAL_SURFACE('',#20530,0.0129);
#4401=CYLINDRICAL_SURFACE('',#20532,0.0129);
#4402=CYLINDRICAL_SURFACE('',#20534,0.0129);
#4403=CYLINDRICAL_SURFACE('',#20536,0.0129);
#4404=CYLINDRICAL_SURFACE('',#20538,0.0129);
#4405=CYLINDRICAL_SURFACE('',#20540,0.0129);
#4406=CYLINDRICAL_SURFACE('',#20542,0.0129);
#4407=CYLINDRICAL_SURFACE('',#20544,0.0129);
#4408=CYLINDRICAL_SURFACE('',#20546,0.0129);
#4409=CYLINDRICAL_SURFACE('',#20548,0.0129);
#4410=CYLINDRICAL_SURFACE('',#20550,0.0129);
#4411=CYLINDRICAL_SURFACE('',#20552,0.0129);
#4412=CYLINDRICAL_SURFACE('',#20554,0.0129);
#4413=CYLINDRICAL_SURFACE('',#20556,0.0129);
#4414=CYLINDRICAL_SURFACE('',#20558,0.0129);
#4415=CYLINDRICAL_SURFACE('',#20560,0.0129);
#4416=CYLINDRICAL_SURFACE('',#20562,0.0129);
#4417=CYLINDRICAL_SURFACE('',#20564,0.0129);
#4418=CYLINDRICAL_SURFACE('',#20566,0.0129);
#4419=CYLINDRICAL_SURFACE('',#20568,0.0129);
#4420=CYLINDRICAL_SURFACE('',#20570,0.0129);
#4421=CYLINDRICAL_SURFACE('',#20572,0.0129);
#4422=CYLINDRICAL_SURFACE('',#20574,0.0129);
#4423=CYLINDRICAL_SURFACE('',#20576,0.0129);
#4424=CYLINDRICAL_SURFACE('',#20578,0.0129);
#4425=CYLINDRICAL_SURFACE('',#20580,0.0129);
#4426=CYLINDRICAL_SURFACE('',#20582,0.0129);
#4427=CYLINDRICAL_SURFACE('',#20584,0.0005);
#4428=CYLINDRICAL_SURFACE('',#20589,0.0129);
#4429=CYLINDRICAL_SURFACE('',#20590,0.0025);
#4430=CYLINDRICAL_SURFACE('',#20593,0.00199999999998973);
#4431=CYLINDRICAL_SURFACE('',#20597,0.0251250000000126);
#4432=CYLINDRICAL_SURFACE('',#20603,0.00200000000001397);
#4433=CYLINDRICAL_SURFACE('',#20608,0.00199999999998997);
#4434=CYLINDRICAL_SURFACE('',#20612,0.0251250000000138);
#4435=CYLINDRICAL_SURFACE('',#20618,0.00199999999999762);
#4436=CYLINDRICAL_SURFACE('',#20623,0.00200000000001296);
#4437=CYLINDRICAL_SURFACE('',#20627,0.0251250000000138);
#4438=CYLINDRICAL_SURFACE('',#20637,0.00199999999998998);
#4439=CYLINDRICAL_SURFACE('',#20641,0.0251250000000291);
#4440=CYLINDRICAL_SURFACE('',#20647,0.00200000000000295);
#4441=CYLINDRICAL_SURFACE('',#20651,0.00199999999998605);
#4442=CYLINDRICAL_SURFACE('',#20685,0.003);
#4443=CYLINDRICAL_SURFACE('',#20687,0.003);
#4444=CYLINDRICAL_SURFACE('',#20692,0.003);
#4445=CYLINDRICAL_SURFACE('',#20694,0.003);
#4446=CYLINDRICAL_SURFACE('',#20696,0.002);
#4447=CYLINDRICAL_SURFACE('',#20706,0.002);
#4448=CYLINDRICAL_SURFACE('',#20715,0.0005);
#4449=CYLINDRICAL_SURFACE('',#20719,0.0005);
#4450=CYLINDRICAL_SURFACE('',#20723,0.0005);
#4451=CYLINDRICAL_SURFACE('',#20727,0.0005);
#4452=CYLINDRICAL_SURFACE('',#20734,0.0045);
#4453=CYLINDRICAL_SURFACE('',#20738,0.00347964100813058);
#4454=CYLINDRICAL_SURFACE('',#20742,0.00347964100813058);
#4455=CYLINDRICAL_SURFACE('',#20746,0.00347964100813058);
#4456=CYLINDRICAL_SURFACE('',#20752,0.00347964100813058);
#4457=CYLINDRICAL_SURFACE('',#20763,0.013);
#4458=CYLINDRICAL_SURFACE('',#20768,0.008);
#4459=CYLINDRICAL_SURFACE('',#20772,0.0017);
#4460=CYLINDRICAL_SURFACE('',#20775,0.0017);
#4461=CYLINDRICAL_SURFACE('',#20778,0.0017);
#4462=CYLINDRICAL_SURFACE('',#20781,0.0017);
#4463=CYLINDRICAL_SURFACE('',#20783,0.006);
#4464=CYLINDRICAL_SURFACE('',#20798,0.008);
#4465=CYLINDRICAL_SURFACE('',#20808,0.00616666666666666);
#4466=CYLINDRICAL_SURFACE('',#20812,0.0005);
#4467=CYLINDRICAL_SURFACE('',#20825,0.0005);
#4468=CYLINDRICAL_SURFACE('',#20834,0.00425);
#4469=CYLINDRICAL_SURFACE('',#20837,0.000585);
#4470=CYLINDRICAL_SURFACE('',#20841,0.00195);
#4471=CYLINDRICAL_SURFACE('',#20844,0.000117);
#4472=CYLINDRICAL_SURFACE('',#20848,0.000468);
#4473=CYLINDRICAL_SURFACE('',#20851,0.00312);
#4474=CYLINDRICAL_SURFACE('',#20854,0.000312);
#4475=CYLINDRICAL_SURFACE('',#20858,0.00039);
#4476=CYLINDRICAL_SURFACE('',#20862,0.000312);
#4477=CYLINDRICAL_SURFACE('',#20865,0.00312);
#4478=CYLINDRICAL_SURFACE('',#20868,0.000468);
#4479=CYLINDRICAL_SURFACE('',#20872,0.000117);
#4480=CYLINDRICAL_SURFACE('',#20875,0.00195);
#4481=CYLINDRICAL_SURFACE('',#20879,0.000585);
#4482=CYLINDRICAL_SURFACE('',#20885,0.00025);
#4483=CYLINDRICAL_SURFACE('',#20888,0.01345);
#4484=CYLINDRICAL_SURFACE('',#20891,0.00025);
#4485=CYLINDRICAL_SURFACE('',#20895,0.00025);
#4486=CYLINDRICAL_SURFACE('',#20898,0.01345);
#4487=CYLINDRICAL_SURFACE('',#20901,0.00025);
#4488=CYLINDRICAL_SURFACE('',#20905,0.00025);
#4489=CYLINDRICAL_SURFACE('',#20908,0.01345);
#4490=CYLINDRICAL_SURFACE('',#20911,0.00025);
#4491=CYLINDRICAL_SURFACE('',#20915,0.00025);
#4492=CYLINDRICAL_SURFACE('',#20918,0.01345);
#4493=CYLINDRICAL_SURFACE('',#20921,0.00025);
#4494=CYLINDRICAL_SURFACE('',#20925,0.00025);
#4495=CYLINDRICAL_SURFACE('',#20928,0.01345);
#4496=CYLINDRICAL_SURFACE('',#20931,0.00025);
#4497=CYLINDRICAL_SURFACE('',#20939,0.013);
#4498=CYLINDRICAL_SURFACE('',#20942,0.013);
#4499=CYLINDRICAL_SURFACE('',#20951,0.013);
#4500=CYLINDRICAL_SURFACE('',#20953,0.013);
#4501=CYLINDRICAL_SURFACE('',#20956,0.013);
#4502=CYLINDRICAL_SURFACE('',#20959,0.0139);
#4503=CYLINDRICAL_SURFACE('',#20962,0.013);
#4504=CYLINDRICAL_SURFACE('',#20966,0.00200000000000295);
#4505=CYLINDRICAL_SURFACE('',#20970,0.0251250000000291);
#4506=CYLINDRICAL_SURFACE('',#20975,0.00200000000001397);
#4507=CYLINDRICAL_SURFACE('',#20979,0.0251250000000126);
#4508=CYLINDRICAL_SURFACE('',#20984,0.00199999999999762);
#4509=CYLINDRICAL_SURFACE('',#20988,0.0251250000000138);
#4510=CYLINDRICAL_SURFACE('',#20993,0.00199999999998605);
#4511=CYLINDRICAL_SURFACE('',#20997,0.0251250000000138);
#4512=CYLINDRICAL_SURFACE('',#21002,0.00199999999998998);
#4513=CYLINDRICAL_SURFACE('',#21006,0.00199999999998973);
#4514=CYLINDRICAL_SURFACE('',#21010,0.00199999999998997);
#4515=CYLINDRICAL_SURFACE('',#21014,0.00200000000001296);
#4516=CYLINDRICAL_SURFACE('',#21056,0.0109);
#4517=CYLINDRICAL_SURFACE('',#21060,0.0045);
#4518=CYLINDRICAL_SURFACE('',#21071,0.013);
#4519=CYLINDRICAL_SURFACE('',#21075,0.008);
#4520=CYLINDRICAL_SURFACE('',#21077,0.0012295);
#4521=CYLINDRICAL_SURFACE('',#21078,0.0012295);
#4522=CYLINDRICAL_SURFACE('',#21079,0.0012295);
#4523=CYLINDRICAL_SURFACE('',#21080,0.0012295);
#4524=CYLINDRICAL_SURFACE('',#21081,0.006);
#4525=CYLINDRICAL_SURFACE('',#21090,0.00025);
#4526=CYLINDRICAL_SURFACE('',#21093,0.01345);
#4527=CYLINDRICAL_SURFACE('',#21096,0.00025);
#4528=CYLINDRICAL_SURFACE('',#21100,0.00025);
#4529=CYLINDRICAL_SURFACE('',#21103,0.01345);
#4530=CYLINDRICAL_SURFACE('',#21106,0.00025);
#4531=CYLINDRICAL_SURFACE('',#21110,0.00025);
#4532=CYLINDRICAL_SURFACE('',#21113,0.01345);
#4533=CYLINDRICAL_SURFACE('',#21116,0.00025);
#4534=CYLINDRICAL_SURFACE('',#21120,0.00025);
#4535=CYLINDRICAL_SURFACE('',#21123,0.01345);
#4536=CYLINDRICAL_SURFACE('',#21126,0.00025);
#4537=CYLINDRICAL_SURFACE('',#21130,0.00025);
#4538=CYLINDRICAL_SURFACE('',#21133,0.01345);
#4539=CYLINDRICAL_SURFACE('',#21136,0.00025);
#4540=CYLINDRICAL_SURFACE('',#21144,0.013);
#4541=CYLINDRICAL_SURFACE('',#21147,0.013);
#4542=CYLINDRICAL_SURFACE('',#21156,0.013);
#4543=CYLINDRICAL_SURFACE('',#21158,0.013);
#4544=CYLINDRICAL_SURFACE('',#21161,0.013);
#4545=CYLINDRICAL_SURFACE('',#21164,0.0139);
#4546=CYLINDRICAL_SURFACE('',#21167,0.013);
#4547=CYLINDRICAL_SURFACE('',#21178,0.002);
#4548=CYLINDRICAL_SURFACE('',#21185,0.0025);
#4549=CYLINDRICAL_SURFACE('',#21189,0.0025);
#4550=CYLINDRICAL_SURFACE('',#21209,0.013);
#4551=CYLINDRICAL_SURFACE('',#21216,0.00075);
#4552=CYLINDRICAL_SURFACE('',#21219,0.00075);
#4553=CYLINDRICAL_SURFACE('',#21222,0.00075);
#4554=CYLINDRICAL_SURFACE('',#21225,0.00075);
#4555=CYLINDRICAL_SURFACE('',#21228,0.0006);
#4556=CYLINDRICAL_SURFACE('',#21231,0.0006);
#4557=CYLINDRICAL_SURFACE('',#21234,0.0006);
#4558=CYLINDRICAL_SURFACE('',#21237,0.0006);
#4559=CYLINDRICAL_SURFACE('',#21240,0.0006);
#4560=CYLINDRICAL_SURFACE('',#21243,0.0006);
#4561=CYLINDRICAL_SURFACE('',#21253,0.01375);
#4562=CYLINDRICAL_SURFACE('',#21263,0.0005);
#4563=CYLINDRICAL_SURFACE('',#21273,0.00025);
#4564=CYLINDRICAL_SURFACE('',#21276,0.01345);
#4565=CYLINDRICAL_SURFACE('',#21279,0.00025);
#4566=CYLINDRICAL_SURFACE('',#21283,0.00025);
#4567=CYLINDRICAL_SURFACE('',#21286,0.01345);
#4568=CYLINDRICAL_SURFACE('',#21289,0.00025);
#4569=CYLINDRICAL_SURFACE('',#21293,0.00025);
#4570=CYLINDRICAL_SURFACE('',#21296,0.01345);
#4571=CYLINDRICAL_SURFACE('',#21299,0.00025);
#4572=CYLINDRICAL_SURFACE('',#21303,0.00025);
#4573=CYLINDRICAL_SURFACE('',#21306,0.01345);
#4574=CYLINDRICAL_SURFACE('',#21309,0.00025);
#4575=CYLINDRICAL_SURFACE('',#21313,0.00025);
#4576=CYLINDRICAL_SURFACE('',#21316,0.01345);
#4577=CYLINDRICAL_SURFACE('',#21319,0.00025);
#4578=CYLINDRICAL_SURFACE('',#21327,0.013);
#4579=CYLINDRICAL_SURFACE('',#21330,0.013);
#4580=CYLINDRICAL_SURFACE('',#21339,0.013);
#4581=CYLINDRICAL_SURFACE('',#21341,0.013);
#4582=CYLINDRICAL_SURFACE('',#21344,0.013);
#4583=CYLINDRICAL_SURFACE('',#21346,0.0139);
#4584=CYLINDRICAL_SURFACE('',#21349,0.013);
#4585=CYLINDRICAL_SURFACE('',#21357,0.0025);
#4586=CYLINDRICAL_SURFACE('',#21359,0.003875);
#4587=CYLINDRICAL_SURFACE('',#21367,0.0005);
#4588=CYLINDRICAL_SURFACE('',#21375,0.0005);
#4589=CYLINDRICAL_SURFACE('',#21378,0.0005);
#4590=CYLINDRICAL_SURFACE('',#21381,0.0005);
#4591=CYLINDRICAL_SURFACE('',#21384,0.0005);
#4592=CYLINDRICAL_SURFACE('',#21387,0.0005);
#4593=CYLINDRICAL_SURFACE('',#21390,0.0005);
#4594=CYLINDRICAL_SURFACE('',#21393,0.0005);
#4595=CYLINDRICAL_SURFACE('',#21396,0.0005);
#4596=CYLINDRICAL_SURFACE('',#21399,0.0005);
#4597=CYLINDRICAL_SURFACE('',#21402,0.0005);
#4598=CYLINDRICAL_SURFACE('',#21405,0.0005);
#4599=CYLINDRICAL_SURFACE('',#21408,0.0005);
#4600=CYLINDRICAL_SURFACE('',#21411,0.0005);
#4601=CYLINDRICAL_SURFACE('',#21414,0.0005);
#4602=CYLINDRICAL_SURFACE('',#21417,0.0005);
#4603=CYLINDRICAL_SURFACE('',#21420,0.0005);
#4604=CYLINDRICAL_SURFACE('',#21423,0.0005);
#4605=CYLINDRICAL_SURFACE('',#21426,0.0005);
#4606=CYLINDRICAL_SURFACE('',#21429,0.0005);
#4607=CYLINDRICAL_SURFACE('',#21432,0.0005);
#4608=CYLINDRICAL_SURFACE('',#21435,0.0005);
#4609=CYLINDRICAL_SURFACE('',#21438,0.0005);
#4610=CYLINDRICAL_SURFACE('',#21441,0.0005);
#4611=CYLINDRICAL_SURFACE('',#21444,0.0005);
#4612=CYLINDRICAL_SURFACE('',#21447,0.0005);
#4613=CYLINDRICAL_SURFACE('',#21450,0.0005);
#4614=CYLINDRICAL_SURFACE('',#21453,0.0005);
#4615=CYLINDRICAL_SURFACE('',#21456,0.0005);
#4616=CYLINDRICAL_SURFACE('',#21459,0.0005);
#4617=CYLINDRICAL_SURFACE('',#21462,0.0005);
#4618=CYLINDRICAL_SURFACE('',#21465,0.0005);
#4619=CYLINDRICAL_SURFACE('',#21468,0.0005);
#4620=CYLINDRICAL_SURFACE('',#21471,0.0005);
#4621=CYLINDRICAL_SURFACE('',#21474,0.0005);
#4622=CYLINDRICAL_SURFACE('',#21477,0.0005);
#4623=CYLINDRICAL_SURFACE('',#21480,0.0005);
#4624=CYLINDRICAL_SURFACE('',#21483,0.0005);
#4625=CYLINDRICAL_SURFACE('',#21486,0.0005);
#4626=CYLINDRICAL_SURFACE('',#21489,0.0005);
#4627=CYLINDRICAL_SURFACE('',#21492,0.0005);
#4628=CYLINDRICAL_SURFACE('',#21495,0.0005);
#4629=CYLINDRICAL_SURFACE('',#21498,0.0005);
#4630=CYLINDRICAL_SURFACE('',#21501,0.0005);
#4631=CYLINDRICAL_SURFACE('',#21504,0.0005);
#4632=CYLINDRICAL_SURFACE('',#21555,0.0129);
#4633=CYLINDRICAL_SURFACE('',#21557,0.0129);
#4634=CYLINDRICAL_SURFACE('',#21559,0.0129);
#4635=CYLINDRICAL_SURFACE('',#21561,0.0129);
#4636=CYLINDRICAL_SURFACE('',#21563,0.0129);
#4637=CYLINDRICAL_SURFACE('',#21565,0.0129);
#4638=CYLINDRICAL_SURFACE('',#21567,0.0129);
#4639=CYLINDRICAL_SURFACE('',#21569,0.0129);
#4640=CYLINDRICAL_SURFACE('',#21571,0.0129);
#4641=CYLINDRICAL_SURFACE('',#21573,0.0129);
#4642=CYLINDRICAL_SURFACE('',#21575,0.0129);
#4643=CYLINDRICAL_SURFACE('',#21577,0.0129);
#4644=CYLINDRICAL_SURFACE('',#21579,0.0129);
#4645=CYLINDRICAL_SURFACE('',#21581,0.0129);
#4646=CYLINDRICAL_SURFACE('',#21583,0.0129);
#4647=CYLINDRICAL_SURFACE('',#21585,0.0129);
#4648=CYLINDRICAL_SURFACE('',#21587,0.0129);
#4649=CYLINDRICAL_SURFACE('',#21589,0.0129);
#4650=CYLINDRICAL_SURFACE('',#21591,0.0129);
#4651=CYLINDRICAL_SURFACE('',#21593,0.0129);
#4652=CYLINDRICAL_SURFACE('',#21595,0.0129);
#4653=CYLINDRICAL_SURFACE('',#21597,0.0129);
#4654=CYLINDRICAL_SURFACE('',#21599,0.0129);
#4655=CYLINDRICAL_SURFACE('',#21601,0.0129);
#4656=CYLINDRICAL_SURFACE('',#21603,0.0129);
#4657=CYLINDRICAL_SURFACE('',#21605,0.0129);
#4658=CYLINDRICAL_SURFACE('',#21607,0.0129);
#4659=CYLINDRICAL_SURFACE('',#21609,0.0129);
#4660=CYLINDRICAL_SURFACE('',#21611,0.0129);
#4661=CYLINDRICAL_SURFACE('',#21613,0.0129);
#4662=CYLINDRICAL_SURFACE('',#21615,0.0129);
#4663=CYLINDRICAL_SURFACE('',#21617,0.0129);
#4664=CYLINDRICAL_SURFACE('',#21619,0.0129);
#4665=CYLINDRICAL_SURFACE('',#21621,0.0129);
#4666=CYLINDRICAL_SURFACE('',#21623,0.0129);
#4667=CYLINDRICAL_SURFACE('',#21625,0.0129);
#4668=CYLINDRICAL_SURFACE('',#21627,0.0129);
#4669=CYLINDRICAL_SURFACE('',#21629,0.0129);
#4670=CYLINDRICAL_SURFACE('',#21631,0.0129);
#4671=CYLINDRICAL_SURFACE('',#21633,0.0129);
#4672=CYLINDRICAL_SURFACE('',#21635,0.0129);
#4673=CYLINDRICAL_SURFACE('',#21637,0.0129);
#4674=CYLINDRICAL_SURFACE('',#21639,0.0129);
#4675=CYLINDRICAL_SURFACE('',#21641,0.0129);
#4676=CYLINDRICAL_SURFACE('',#21643,0.0005);
#4677=CYLINDRICAL_SURFACE('',#21648,0.0129);
#4678=CYLINDRICAL_SURFACE('',#21649,0.0025);
#4679=CYLINDRICAL_SURFACE('',#21656,0.0025);
#4680=CYLINDRICAL_SURFACE('',#21666,0.00433333333333334);
#4681=CYLINDRICAL_SURFACE('',#21668,0.00025);
#4682=CYLINDRICAL_SURFACE('',#21671,0.01345);
#4683=CYLINDRICAL_SURFACE('',#21674,0.00025);
#4684=CYLINDRICAL_SURFACE('',#21678,0.00025);
#4685=CYLINDRICAL_SURFACE('',#21681,0.01345);
#4686=CYLINDRICAL_SURFACE('',#21684,0.00025);
#4687=CYLINDRICAL_SURFACE('',#21688,0.00025);
#4688=CYLINDRICAL_SURFACE('',#21691,0.01345);
#4689=CYLINDRICAL_SURFACE('',#21694,0.00025);
#4690=CYLINDRICAL_SURFACE('',#21698,0.00025);
#4691=CYLINDRICAL_SURFACE('',#21701,0.01345);
#4692=CYLINDRICAL_SURFACE('',#21704,0.00025);
#4693=CYLINDRICAL_SURFACE('',#21708,0.00025);
#4694=CYLINDRICAL_SURFACE('',#21711,0.01345);
#4695=CYLINDRICAL_SURFACE('',#21714,0.00025);
#4696=CYLINDRICAL_SURFACE('',#21722,0.013);
#4697=CYLINDRICAL_SURFACE('',#21725,0.013);
#4698=CYLINDRICAL_SURFACE('',#21734,0.013);
#4699=CYLINDRICAL_SURFACE('',#21736,0.013);
#4700=CYLINDRICAL_SURFACE('',#21739,0.013);
#4701=CYLINDRICAL_SURFACE('',#21742,0.0139);
#4702=CYLINDRICAL_SURFACE('',#21745,0.013);
#4703=CYLINDRICAL_SURFACE('',#21754,0.0005);
#4704=CYLINDRICAL_SURFACE('',#21761,0.002);
#4705=CYLINDRICAL_SURFACE('',#21765,0.002);
#4706=CYLINDRICAL_SURFACE('',#21768,0.025125);
#4707=CYLINDRICAL_SURFACE('',#21771,0.002);
#4708=CYLINDRICAL_SURFACE('',#21775,0.002);
#4709=CYLINDRICAL_SURFACE('',#21778,0.025125);
#4710=CYLINDRICAL_SURFACE('',#21781,0.002);
#4711=CYLINDRICAL_SURFACE('',#21785,0.002);
#4712=CYLINDRICAL_SURFACE('',#21788,0.025125);
#4713=CYLINDRICAL_SURFACE('',#21791,0.002);
#4714=CYLINDRICAL_SURFACE('',#21795,0.002);
#4715=CYLINDRICAL_SURFACE('',#21804,0.025125);
#4716=CYLINDRICAL_SURFACE('',#21806,0.0017);
#4717=CYLINDRICAL_SURFACE('',#21808,0.0017);
#4718=CYLINDRICAL_SURFACE('',#21810,0.0017);
#4719=CYLINDRICAL_SURFACE('',#21812,0.0017);
#4720=CYLINDRICAL_SURFACE('',#21824,0.00025);
#4721=CYLINDRICAL_SURFACE('',#21827,0.01345);
#4722=CYLINDRICAL_SURFACE('',#21830,0.00025);
#4723=CYLINDRICAL_SURFACE('',#21834,0.00025);
#4724=CYLINDRICAL_SURFACE('',#21837,0.01345);
#4725=CYLINDRICAL_SURFACE('',#21840,0.00025);
#4726=CYLINDRICAL_SURFACE('',#21844,0.00025);
#4727=CYLINDRICAL_SURFACE('',#21847,0.01345);
#4728=CYLINDRICAL_SURFACE('',#21850,0.00025);
#4729=CYLINDRICAL_SURFACE('',#21854,0.00025);
#4730=CYLINDRICAL_SURFACE('',#21857,0.01345);
#4731=CYLINDRICAL_SURFACE('',#21860,0.00025);
#4732=CYLINDRICAL_SURFACE('',#21864,0.00025);
#4733=CYLINDRICAL_SURFACE('',#21867,0.01345);
#4734=CYLINDRICAL_SURFACE('',#21870,0.00025);
#4735=CYLINDRICAL_SURFACE('',#21878,0.013);
#4736=CYLINDRICAL_SURFACE('',#21881,0.013);
#4737=CYLINDRICAL_SURFACE('',#21890,0.013);
#4738=CYLINDRICAL_SURFACE('',#21892,0.013);
#4739=CYLINDRICAL_SURFACE('',#21895,0.013);
#4740=CYLINDRICAL_SURFACE('',#21897,0.0139);
#4741=CYLINDRICAL_SURFACE('',#21900,0.013);
#4742=CYLINDRICAL_SURFACE('',#21960,0.0025);
#4743=CYLINDRICAL_SURFACE('',#21963,0.012);
#4744=CYLINDRICAL_SURFACE('',#21969,0.00025);
#4745=CYLINDRICAL_SURFACE('',#21972,0.01345);
#4746=CYLINDRICAL_SURFACE('',#21975,0.00025);
#4747=CYLINDRICAL_SURFACE('',#21979,0.00025);
#4748=CYLINDRICAL_SURFACE('',#21982,0.01345);
#4749=CYLINDRICAL_SURFACE('',#21985,0.00025);
#4750=CYLINDRICAL_SURFACE('',#21989,0.00025);
#4751=CYLINDRICAL_SURFACE('',#21992,0.01345);
#4752=CYLINDRICAL_SURFACE('',#21995,0.00025);
#4753=CYLINDRICAL_SURFACE('',#21999,0.00025);
#4754=CYLINDRICAL_SURFACE('',#22002,0.01345);
#4755=CYLINDRICAL_SURFACE('',#22005,0.00025);
#4756=CYLINDRICAL_SURFACE('',#22009,0.00025);
#4757=CYLINDRICAL_SURFACE('',#22012,0.01345);
#4758=CYLINDRICAL_SURFACE('',#22015,0.00025);
#4759=CYLINDRICAL_SURFACE('',#22023,0.013);
#4760=CYLINDRICAL_SURFACE('',#22026,0.013);
#4761=CYLINDRICAL_SURFACE('',#22035,0.013);
#4762=CYLINDRICAL_SURFACE('',#22037,0.013);
#4763=CYLINDRICAL_SURFACE('',#22040,0.013);
#4764=CYLINDRICAL_SURFACE('',#22043,0.0139);
#4765=CYLINDRICAL_SURFACE('',#22046,0.013);
#4766=CYLINDRICAL_SURFACE('',#22050,0.00025);
#4767=CYLINDRICAL_SURFACE('',#22053,0.01345);
#4768=CYLINDRICAL_SURFACE('',#22056,0.00025);
#4769=CYLINDRICAL_SURFACE('',#22060,0.00025);
#4770=CYLINDRICAL_SURFACE('',#22063,0.01345);
#4771=CYLINDRICAL_SURFACE('',#22066,0.00025);
#4772=CYLINDRICAL_SURFACE('',#22070,0.00025);
#4773=CYLINDRICAL_SURFACE('',#22073,0.01345);
#4774=CYLINDRICAL_SURFACE('',#22076,0.00025);
#4775=CYLINDRICAL_SURFACE('',#22080,0.00025);
#4776=CYLINDRICAL_SURFACE('',#22083,0.01345);
#4777=CYLINDRICAL_SURFACE('',#22086,0.00025);
#4778=CYLINDRICAL_SURFACE('',#22090,0.00025);
#4779=CYLINDRICAL_SURFACE('',#22093,0.01345);
#4780=CYLINDRICAL_SURFACE('',#22096,0.00025);
#4781=CYLINDRICAL_SURFACE('',#22104,0.013);
#4782=CYLINDRICAL_SURFACE('',#22107,0.013);
#4783=CYLINDRICAL_SURFACE('',#22116,0.013);
#4784=CYLINDRICAL_SURFACE('',#22118,0.013);
#4785=CYLINDRICAL_SURFACE('',#22121,0.013);
#4786=CYLINDRICAL_SURFACE('',#22124,0.0139);
#4787=CYLINDRICAL_SURFACE('',#22127,0.013);
#4788=CYLINDRICAL_SURFACE('',#22136,0.0025);
#4789=CYLINDRICAL_SURFACE('',#22146,0.00433333333333334);
#4790=CYLINDRICAL_SURFACE('',#22150,0.0005);
#4791=CYLINDRICAL_SURFACE('',#22164,0.0015);
#4792=CYLINDRICAL_SURFACE('',#22217,0.001364685);
#4793=FACE_OUTER_BOUND('',#5838,.T.);
#4794=FACE_OUTER_BOUND('',#5839,.T.);
#4795=FACE_OUTER_BOUND('',#5840,.T.);
#4796=FACE_OUTER_BOUND('',#5842,.T.);
#4797=FACE_OUTER_BOUND('',#5843,.T.);
#4798=FACE_OUTER_BOUND('',#5845,.T.);
#4799=FACE_OUTER_BOUND('',#5846,.T.);
#4800=FACE_OUTER_BOUND('',#5847,.T.);
#4801=FACE_OUTER_BOUND('',#5848,.T.);
#4802=FACE_OUTER_BOUND('',#5849,.T.);
#4803=FACE_OUTER_BOUND('',#5850,.T.);
#4804=FACE_OUTER_BOUND('',#5851,.T.);
#4805=FACE_OUTER_BOUND('',#5852,.T.);
#4806=FACE_OUTER_BOUND('',#5853,.T.);
#4807=FACE_OUTER_BOUND('',#5854,.T.);
#4808=FACE_OUTER_BOUND('',#5855,.T.);
#4809=FACE_OUTER_BOUND('',#5856,.T.);
#4810=FACE_OUTER_BOUND('',#5857,.T.);
#4811=FACE_OUTER_BOUND('',#5858,.T.);
#4812=FACE_OUTER_BOUND('',#5859,.T.);
#4813=FACE_OUTER_BOUND('',#5860,.T.);
#4814=FACE_OUTER_BOUND('',#5861,.T.);
#4815=FACE_OUTER_BOUND('',#5862,.T.);
#4816=FACE_OUTER_BOUND('',#5863,.T.);
#4817=FACE_OUTER_BOUND('',#5864,.T.);
#4818=FACE_OUTER_BOUND('',#5865,.T.);
#4819=FACE_OUTER_BOUND('',#5866,.T.);
#4820=FACE_OUTER_BOUND('',#5867,.T.);
#4821=FACE_OUTER_BOUND('',#5868,.T.);
#4822=FACE_OUTER_BOUND('',#5869,.T.);
#4823=FACE_OUTER_BOUND('',#5870,.T.);
#4824=FACE_OUTER_BOUND('',#5871,.T.);
#4825=FACE_OUTER_BOUND('',#5872,.T.);
#4826=FACE_OUTER_BOUND('',#5873,.T.);
#4827=FACE_OUTER_BOUND('',#5874,.T.);
#4828=FACE_OUTER_BOUND('',#5875,.T.);
#4829=FACE_OUTER_BOUND('',#5876,.T.);
#4830=FACE_OUTER_BOUND('',#5877,.T.);
#4831=FACE_OUTER_BOUND('',#5878,.T.);
#4832=FACE_OUTER_BOUND('',#5879,.T.);
#4833=FACE_OUTER_BOUND('',#5880,.T.);
#4834=FACE_OUTER_BOUND('',#5881,.T.);
#4835=FACE_OUTER_BOUND('',#5882,.T.);
#4836=FACE_OUTER_BOUND('',#5884,.T.);
#4837=FACE_OUTER_BOUND('',#5885,.T.);
#4838=FACE_OUTER_BOUND('',#5886,.T.);
#4839=FACE_OUTER_BOUND('',#5888,.T.);
#4840=FACE_OUTER_BOUND('',#5890,.T.);
#4841=FACE_OUTER_BOUND('',#5891,.T.);
#4842=FACE_OUTER_BOUND('',#5892,.T.);
#4843=FACE_OUTER_BOUND('',#5893,.T.);
#4844=FACE_OUTER_BOUND('',#5894,.T.);
#4845=FACE_OUTER_BOUND('',#5895,.T.);
#4846=FACE_OUTER_BOUND('',#5896,.T.);
#4847=FACE_OUTER_BOUND('',#5897,.T.);
#4848=FACE_OUTER_BOUND('',#5898,.T.);
#4849=FACE_OUTER_BOUND('',#5899,.T.);
#4850=FACE_OUTER_BOUND('',#5900,.T.);
#4851=FACE_OUTER_BOUND('',#5901,.T.);
#4852=FACE_OUTER_BOUND('',#5902,.T.);
#4853=FACE_OUTER_BOUND('',#5903,.T.);
#4854=FACE_OUTER_BOUND('',#5905,.T.);
#4855=FACE_OUTER_BOUND('',#5906,.T.);
#4856=FACE_OUTER_BOUND('',#5907,.T.);
#4857=FACE_OUTER_BOUND('',#5908,.T.);
#4858=FACE_OUTER_BOUND('',#5909,.T.);
#4859=FACE_OUTER_BOUND('',#5910,.T.);
#4860=FACE_OUTER_BOUND('',#5911,.T.);
#4861=FACE_OUTER_BOUND('',#5912,.T.);
#4862=FACE_OUTER_BOUND('',#5913,.T.);
#4863=FACE_OUTER_BOUND('',#5914,.T.);
#4864=FACE_OUTER_BOUND('',#5915,.T.);
#4865=FACE_OUTER_BOUND('',#5916,.T.);
#4866=FACE_OUTER_BOUND('',#5917,.T.);
#4867=FACE_OUTER_BOUND('',#5918,.T.);
#4868=FACE_OUTER_BOUND('',#5920,.T.);
#4869=FACE_OUTER_BOUND('',#5921,.T.);
#4870=FACE_OUTER_BOUND('',#5922,.T.);
#4871=FACE_OUTER_BOUND('',#5923,.T.);
#4872=FACE_OUTER_BOUND('',#5924,.T.);
#4873=FACE_OUTER_BOUND('',#5925,.T.);
#4874=FACE_OUTER_BOUND('',#5926,.T.);
#4875=FACE_OUTER_BOUND('',#5927,.T.);
#4876=FACE_OUTER_BOUND('',#5928,.T.);
#4877=FACE_OUTER_BOUND('',#5929,.T.);
#4878=FACE_OUTER_BOUND('',#5930,.T.);
#4879=FACE_OUTER_BOUND('',#5931,.T.);
#4880=FACE_OUTER_BOUND('',#5932,.T.);
#4881=FACE_OUTER_BOUND('',#5933,.T.);
#4882=FACE_OUTER_BOUND('',#5935,.T.);
#4883=FACE_OUTER_BOUND('',#5936,.T.);
#4884=FACE_OUTER_BOUND('',#5937,.T.);
#4885=FACE_OUTER_BOUND('',#5938,.T.);
#4886=FACE_OUTER_BOUND('',#5939,.T.);
#4887=FACE_OUTER_BOUND('',#5940,.T.);
#4888=FACE_OUTER_BOUND('',#5941,.T.);
#4889=FACE_OUTER_BOUND('',#5942,.T.);
#4890=FACE_OUTER_BOUND('',#5943,.T.);
#4891=FACE_OUTER_BOUND('',#5944,.T.);
#4892=FACE_OUTER_BOUND('',#5945,.T.);
#4893=FACE_OUTER_BOUND('',#5946,.T.);
#4894=FACE_OUTER_BOUND('',#5947,.T.);
#4895=FACE_OUTER_BOUND('',#5948,.T.);
#4896=FACE_OUTER_BOUND('',#5950,.T.);
#4897=FACE_OUTER_BOUND('',#5951,.T.);
#4898=FACE_OUTER_BOUND('',#5952,.T.);
#4899=FACE_OUTER_BOUND('',#5953,.T.);
#4900=FACE_OUTER_BOUND('',#5954,.T.);
#4901=FACE_OUTER_BOUND('',#5955,.T.);
#4902=FACE_OUTER_BOUND('',#5956,.T.);
#4903=FACE_OUTER_BOUND('',#5957,.T.);
#4904=FACE_OUTER_BOUND('',#5958,.T.);
#4905=FACE_OUTER_BOUND('',#5959,.T.);
#4906=FACE_OUTER_BOUND('',#5960,.T.);
#4907=FACE_OUTER_BOUND('',#5961,.T.);
#4908=FACE_OUTER_BOUND('',#5962,.T.);
#4909=FACE_OUTER_BOUND('',#5963,.T.);
#4910=FACE_OUTER_BOUND('',#5965,.T.);
#4911=FACE_OUTER_BOUND('',#5966,.T.);
#4912=FACE_OUTER_BOUND('',#5967,.T.);
#4913=FACE_OUTER_BOUND('',#5968,.T.);
#4914=FACE_OUTER_BOUND('',#5969,.T.);
#4915=FACE_OUTER_BOUND('',#5970,.T.);
#4916=FACE_OUTER_BOUND('',#5971,.T.);
#4917=FACE_OUTER_BOUND('',#5972,.T.);
#4918=FACE_OUTER_BOUND('',#5973,.T.);
#4919=FACE_OUTER_BOUND('',#5974,.T.);
#4920=FACE_OUTER_BOUND('',#5975,.T.);
#4921=FACE_OUTER_BOUND('',#5976,.T.);
#4922=FACE_OUTER_BOUND('',#5977,.T.);
#4923=FACE_OUTER_BOUND('',#5978,.T.);
#4924=FACE_OUTER_BOUND('',#5980,.T.);
#4925=FACE_OUTER_BOUND('',#5981,.T.);
#4926=FACE_OUTER_BOUND('',#5982,.T.);
#4927=FACE_OUTER_BOUND('',#5983,.T.);
#4928=FACE_OUTER_BOUND('',#5984,.T.);
#4929=FACE_OUTER_BOUND('',#5985,.T.);
#4930=FACE_OUTER_BOUND('',#5986,.T.);
#4931=FACE_OUTER_BOUND('',#5987,.T.);
#4932=FACE_OUTER_BOUND('',#5988,.T.);
#4933=FACE_OUTER_BOUND('',#5989,.T.);
#4934=FACE_OUTER_BOUND('',#5990,.T.);
#4935=FACE_OUTER_BOUND('',#5991,.T.);
#4936=FACE_OUTER_BOUND('',#5992,.T.);
#4937=FACE_OUTER_BOUND('',#5993,.T.);
#4938=FACE_OUTER_BOUND('',#5995,.T.);
#4939=FACE_OUTER_BOUND('',#5996,.T.);
#4940=FACE_OUTER_BOUND('',#5997,.T.);
#4941=FACE_OUTER_BOUND('',#5998,.T.);
#4942=FACE_OUTER_BOUND('',#5999,.T.);
#4943=FACE_OUTER_BOUND('',#6000,.T.);
#4944=FACE_OUTER_BOUND('',#6001,.T.);
#4945=FACE_OUTER_BOUND('',#6002,.T.);
#4946=FACE_OUTER_BOUND('',#6003,.T.);
#4947=FACE_OUTER_BOUND('',#6004,.T.);
#4948=FACE_OUTER_BOUND('',#6005,.T.);
#4949=FACE_OUTER_BOUND('',#6006,.T.);
#4950=FACE_OUTER_BOUND('',#6007,.T.);
#4951=FACE_OUTER_BOUND('',#6008,.T.);
#4952=FACE_OUTER_BOUND('',#6010,.T.);
#4953=FACE_OUTER_BOUND('',#6011,.T.);
#4954=FACE_OUTER_BOUND('',#6012,.T.);
#4955=FACE_OUTER_BOUND('',#6013,.T.);
#4956=FACE_OUTER_BOUND('',#6014,.T.);
#4957=FACE_OUTER_BOUND('',#6015,.T.);
#4958=FACE_OUTER_BOUND('',#6016,.T.);
#4959=FACE_OUTER_BOUND('',#6017,.T.);
#4960=FACE_OUTER_BOUND('',#6019,.T.);
#4961=FACE_OUTER_BOUND('',#6021,.T.);
#4962=FACE_OUTER_BOUND('',#6023,.T.);
#4963=FACE_OUTER_BOUND('',#6025,.T.);
#4964=FACE_OUTER_BOUND('',#6027,.T.);
#4965=FACE_OUTER_BOUND('',#6029,.T.);
#4966=FACE_OUTER_BOUND('',#6031,.T.);
#4967=FACE_OUTER_BOUND('',#6033,.T.);
#4968=FACE_OUTER_BOUND('',#6034,.T.);
#4969=FACE_OUTER_BOUND('',#6035,.T.);
#4970=FACE_OUTER_BOUND('',#6036,.T.);
#4971=FACE_OUTER_BOUND('',#6037,.T.);
#4972=FACE_OUTER_BOUND('',#6038,.T.);
#4973=FACE_OUTER_BOUND('',#6039,.T.);
#4974=FACE_OUTER_BOUND('',#6040,.T.);
#4975=FACE_OUTER_BOUND('',#6041,.T.);
#4976=FACE_OUTER_BOUND('',#6042,.T.);
#4977=FACE_OUTER_BOUND('',#6043,.T.);
#4978=FACE_OUTER_BOUND('',#6044,.T.);
#4979=FACE_OUTER_BOUND('',#6045,.T.);
#4980=FACE_OUTER_BOUND('',#6046,.T.);
#4981=FACE_OUTER_BOUND('',#6047,.T.);
#4982=FACE_OUTER_BOUND('',#6048,.T.);
#4983=FACE_OUTER_BOUND('',#6049,.T.);
#4984=FACE_OUTER_BOUND('',#6050,.T.);
#4985=FACE_OUTER_BOUND('',#6051,.T.);
#4986=FACE_OUTER_BOUND('',#6052,.T.);
#4987=FACE_OUTER_BOUND('',#6053,.T.);
#4988=FACE_OUTER_BOUND('',#6054,.T.);
#4989=FACE_OUTER_BOUND('',#6055,.T.);
#4990=FACE_OUTER_BOUND('',#6056,.T.);
#4991=FACE_OUTER_BOUND('',#6057,.T.);
#4992=FACE_OUTER_BOUND('',#6058,.T.);
#4993=FACE_OUTER_BOUND('',#6059,.T.);
#4994=FACE_OUTER_BOUND('',#6060,.T.);
#4995=FACE_OUTER_BOUND('',#6061,.T.);
#4996=FACE_OUTER_BOUND('',#6062,.T.);
#4997=FACE_OUTER_BOUND('',#6063,.T.);
#4998=FACE_OUTER_BOUND('',#6064,.T.);
#4999=FACE_OUTER_BOUND('',#6065,.T.);
#5000=FACE_OUTER_BOUND('',#6066,.T.);
#5001=FACE_OUTER_BOUND('',#6067,.T.);
#5002=FACE_OUTER_BOUND('',#6068,.T.);
#5003=FACE_OUTER_BOUND('',#6069,.T.);
#5004=FACE_OUTER_BOUND('',#6070,.T.);
#5005=FACE_OUTER_BOUND('',#6071,.T.);
#5006=FACE_OUTER_BOUND('',#6072,.T.);
#5007=FACE_OUTER_BOUND('',#6073,.T.);
#5008=FACE_OUTER_BOUND('',#6074,.T.);
#5009=FACE_OUTER_BOUND('',#6075,.T.);
#5010=FACE_OUTER_BOUND('',#6076,.T.);
#5011=FACE_OUTER_BOUND('',#6077,.T.);
#5012=FACE_OUTER_BOUND('',#6078,.T.);
#5013=FACE_OUTER_BOUND('',#6079,.T.);
#5014=FACE_OUTER_BOUND('',#6080,.T.);
#5015=FACE_OUTER_BOUND('',#6081,.T.);
#5016=FACE_OUTER_BOUND('',#6082,.T.);
#5017=FACE_OUTER_BOUND('',#6083,.T.);
#5018=FACE_OUTER_BOUND('',#6084,.T.);
#5019=FACE_OUTER_BOUND('',#6085,.T.);
#5020=FACE_OUTER_BOUND('',#6086,.T.);
#5021=FACE_OUTER_BOUND('',#6087,.T.);
#5022=FACE_OUTER_BOUND('',#6088,.T.);
#5023=FACE_OUTER_BOUND('',#6089,.T.);
#5024=FACE_OUTER_BOUND('',#6090,.T.);
#5025=FACE_OUTER_BOUND('',#6092,.T.);
#5026=FACE_OUTER_BOUND('',#6093,.T.);
#5027=FACE_OUTER_BOUND('',#6094,.T.);
#5028=FACE_OUTER_BOUND('',#6095,.T.);
#5029=FACE_OUTER_BOUND('',#6096,.T.);
#5030=FACE_OUTER_BOUND('',#6097,.T.);
#5031=FACE_OUTER_BOUND('',#6098,.T.);
#5032=FACE_OUTER_BOUND('',#6099,.T.);
#5033=FACE_OUTER_BOUND('',#6100,.T.);
#5034=FACE_OUTER_BOUND('',#6101,.T.);
#5035=FACE_OUTER_BOUND('',#6102,.T.);
#5036=FACE_OUTER_BOUND('',#6103,.T.);
#5037=FACE_OUTER_BOUND('',#6104,.T.);
#5038=FACE_OUTER_BOUND('',#6105,.T.);
#5039=FACE_OUTER_BOUND('',#6106,.T.);
#5040=FACE_OUTER_BOUND('',#6107,.T.);
#5041=FACE_OUTER_BOUND('',#6108,.T.);
#5042=FACE_OUTER_BOUND('',#6109,.T.);
#5043=FACE_OUTER_BOUND('',#6110,.T.);
#5044=FACE_OUTER_BOUND('',#6111,.T.);
#5045=FACE_OUTER_BOUND('',#6112,.T.);
#5046=FACE_OUTER_BOUND('',#6113,.T.);
#5047=FACE_OUTER_BOUND('',#6114,.T.);
#5048=FACE_OUTER_BOUND('',#6115,.T.);
#5049=FACE_OUTER_BOUND('',#6116,.T.);
#5050=FACE_OUTER_BOUND('',#6117,.T.);
#5051=FACE_OUTER_BOUND('',#6118,.T.);
#5052=FACE_OUTER_BOUND('',#6119,.T.);
#5053=FACE_OUTER_BOUND('',#6120,.T.);
#5054=FACE_OUTER_BOUND('',#6121,.T.);
#5055=FACE_OUTER_BOUND('',#6122,.T.);
#5056=FACE_OUTER_BOUND('',#6123,.T.);
#5057=FACE_OUTER_BOUND('',#6124,.T.);
#5058=FACE_OUTER_BOUND('',#6125,.T.);
#5059=FACE_OUTER_BOUND('',#6126,.T.);
#5060=FACE_OUTER_BOUND('',#6127,.T.);
#5061=FACE_OUTER_BOUND('',#6128,.T.);
#5062=FACE_OUTER_BOUND('',#6129,.T.);
#5063=FACE_OUTER_BOUND('',#6130,.T.);
#5064=FACE_OUTER_BOUND('',#6131,.T.);
#5065=FACE_OUTER_BOUND('',#6132,.T.);
#5066=FACE_OUTER_BOUND('',#6133,.T.);
#5067=FACE_OUTER_BOUND('',#6134,.T.);
#5068=FACE_OUTER_BOUND('',#6135,.T.);
#5069=FACE_OUTER_BOUND('',#6136,.T.);
#5070=FACE_OUTER_BOUND('',#6137,.T.);
#5071=FACE_OUTER_BOUND('',#6139,.T.);
#5072=FACE_OUTER_BOUND('',#6140,.T.);
#5073=FACE_OUTER_BOUND('',#6141,.T.);
#5074=FACE_OUTER_BOUND('',#6142,.T.);
#5075=FACE_OUTER_BOUND('',#6143,.T.);
#5076=FACE_OUTER_BOUND('',#6144,.T.);
#5077=FACE_OUTER_BOUND('',#6145,.T.);
#5078=FACE_OUTER_BOUND('',#6146,.T.);
#5079=FACE_OUTER_BOUND('',#6147,.T.);
#5080=FACE_OUTER_BOUND('',#6148,.T.);
#5081=FACE_OUTER_BOUND('',#6149,.T.);
#5082=FACE_OUTER_BOUND('',#6150,.T.);
#5083=FACE_OUTER_BOUND('',#6151,.T.);
#5084=FACE_OUTER_BOUND('',#6152,.T.);
#5085=FACE_OUTER_BOUND('',#6153,.T.);
#5086=FACE_OUTER_BOUND('',#6154,.T.);
#5087=FACE_OUTER_BOUND('',#6155,.T.);
#5088=FACE_OUTER_BOUND('',#6156,.T.);
#5089=FACE_OUTER_BOUND('',#6157,.T.);
#5090=FACE_OUTER_BOUND('',#6158,.T.);
#5091=FACE_OUTER_BOUND('',#6159,.T.);
#5092=FACE_OUTER_BOUND('',#6160,.T.);
#5093=FACE_OUTER_BOUND('',#6161,.T.);
#5094=FACE_OUTER_BOUND('',#6162,.T.);
#5095=FACE_OUTER_BOUND('',#6163,.T.);
#5096=FACE_OUTER_BOUND('',#6164,.T.);
#5097=FACE_OUTER_BOUND('',#6165,.T.);
#5098=FACE_OUTER_BOUND('',#6166,.T.);
#5099=FACE_OUTER_BOUND('',#6167,.T.);
#5100=FACE_OUTER_BOUND('',#6168,.T.);
#5101=FACE_OUTER_BOUND('',#6169,.T.);
#5102=FACE_OUTER_BOUND('',#6170,.T.);
#5103=FACE_OUTER_BOUND('',#6171,.T.);
#5104=FACE_OUTER_BOUND('',#6172,.T.);
#5105=FACE_OUTER_BOUND('',#6173,.T.);
#5106=FACE_OUTER_BOUND('',#6174,.T.);
#5107=FACE_OUTER_BOUND('',#6176,.T.);
#5108=FACE_OUTER_BOUND('',#6177,.T.);
#5109=FACE_OUTER_BOUND('',#6178,.T.);
#5110=FACE_OUTER_BOUND('',#6179,.T.);
#5111=FACE_OUTER_BOUND('',#6180,.T.);
#5112=FACE_OUTER_BOUND('',#6181,.T.);
#5113=FACE_OUTER_BOUND('',#6182,.T.);
#5114=FACE_OUTER_BOUND('',#6183,.T.);
#5115=FACE_OUTER_BOUND('',#6188,.T.);
#5116=FACE_OUTER_BOUND('',#6189,.T.);
#5117=FACE_OUTER_BOUND('',#6190,.T.);
#5118=FACE_OUTER_BOUND('',#6191,.T.);
#5119=FACE_OUTER_BOUND('',#6192,.T.);
#5120=FACE_OUTER_BOUND('',#6193,.T.);
#5121=FACE_OUTER_BOUND('',#6194,.T.);
#5122=FACE_OUTER_BOUND('',#6195,.T.);
#5123=FACE_OUTER_BOUND('',#6196,.T.);
#5124=FACE_OUTER_BOUND('',#6197,.T.);
#5125=FACE_OUTER_BOUND('',#6198,.T.);
#5126=FACE_OUTER_BOUND('',#6199,.T.);
#5127=FACE_OUTER_BOUND('',#6200,.T.);
#5128=FACE_OUTER_BOUND('',#6201,.T.);
#5129=FACE_OUTER_BOUND('',#6202,.T.);
#5130=FACE_OUTER_BOUND('',#6203,.T.);
#5131=FACE_OUTER_BOUND('',#6204,.T.);
#5132=FACE_OUTER_BOUND('',#6205,.T.);
#5133=FACE_OUTER_BOUND('',#6206,.T.);
#5134=FACE_OUTER_BOUND('',#6207,.T.);
#5135=FACE_OUTER_BOUND('',#6208,.T.);
#5136=FACE_OUTER_BOUND('',#6209,.T.);
#5137=FACE_OUTER_BOUND('',#6210,.T.);
#5138=FACE_OUTER_BOUND('',#6211,.T.);
#5139=FACE_OUTER_BOUND('',#6212,.T.);
#5140=FACE_OUTER_BOUND('',#6213,.T.);
#5141=FACE_OUTER_BOUND('',#6214,.T.);
#5142=FACE_OUTER_BOUND('',#6215,.T.);
#5143=FACE_OUTER_BOUND('',#6216,.T.);
#5144=FACE_OUTER_BOUND('',#6217,.T.);
#5145=FACE_OUTER_BOUND('',#6218,.T.);
#5146=FACE_OUTER_BOUND('',#6219,.T.);
#5147=FACE_OUTER_BOUND('',#6220,.T.);
#5148=FACE_OUTER_BOUND('',#6221,.T.);
#5149=FACE_OUTER_BOUND('',#6222,.T.);
#5150=FACE_OUTER_BOUND('',#6223,.T.);
#5151=FACE_OUTER_BOUND('',#6225,.T.);
#5152=FACE_OUTER_BOUND('',#6226,.T.);
#5153=FACE_OUTER_BOUND('',#6227,.T.);
#5154=FACE_OUTER_BOUND('',#6228,.T.);
#5155=FACE_OUTER_BOUND('',#6230,.T.);
#5156=FACE_OUTER_BOUND('',#6231,.T.);
#5157=FACE_OUTER_BOUND('',#6233,.T.);
#5158=FACE_OUTER_BOUND('',#6234,.T.);
#5159=FACE_OUTER_BOUND('',#6236,.T.);
#5160=FACE_OUTER_BOUND('',#6237,.T.);
#5161=FACE_OUTER_BOUND('',#6239,.T.);
#5162=FACE_OUTER_BOUND('',#6240,.T.);
#5163=FACE_OUTER_BOUND('',#6243,.T.);
#5164=FACE_OUTER_BOUND('',#6244,.T.);
#5165=FACE_OUTER_BOUND('',#6246,.T.);
#5166=FACE_OUTER_BOUND('',#6248,.T.);
#5167=FACE_OUTER_BOUND('',#6249,.T.);
#5168=FACE_OUTER_BOUND('',#6250,.T.);
#5169=FACE_OUTER_BOUND('',#6251,.T.);
#5170=FACE_OUTER_BOUND('',#6252,.T.);
#5171=FACE_OUTER_BOUND('',#6253,.T.);
#5172=FACE_OUTER_BOUND('',#6254,.T.);
#5173=FACE_OUTER_BOUND('',#6256,.T.);
#5174=FACE_OUTER_BOUND('',#6257,.T.);
#5175=FACE_OUTER_BOUND('',#6259,.T.);
#5176=FACE_OUTER_BOUND('',#6260,.T.);
#5177=FACE_OUTER_BOUND('',#6261,.T.);
#5178=FACE_OUTER_BOUND('',#6262,.T.);
#5179=FACE_OUTER_BOUND('',#6263,.T.);
#5180=FACE_OUTER_BOUND('',#6264,.T.);
#5181=FACE_OUTER_BOUND('',#6265,.T.);
#5182=FACE_OUTER_BOUND('',#6266,.T.);
#5183=FACE_OUTER_BOUND('',#6267,.T.);
#5184=FACE_OUTER_BOUND('',#6268,.T.);
#5185=FACE_OUTER_BOUND('',#6269,.T.);
#5186=FACE_OUTER_BOUND('',#6270,.T.);
#5187=FACE_OUTER_BOUND('',#6271,.T.);
#5188=FACE_OUTER_BOUND('',#6272,.T.);
#5189=FACE_OUTER_BOUND('',#6273,.T.);
#5190=FACE_OUTER_BOUND('',#6274,.T.);
#5191=FACE_OUTER_BOUND('',#6275,.T.);
#5192=FACE_OUTER_BOUND('',#6276,.T.);
#5193=FACE_OUTER_BOUND('',#6277,.T.);
#5194=FACE_OUTER_BOUND('',#6278,.T.);
#5195=FACE_OUTER_BOUND('',#6279,.T.);
#5196=FACE_OUTER_BOUND('',#6280,.T.);
#5197=FACE_OUTER_BOUND('',#6281,.T.);
#5198=FACE_OUTER_BOUND('',#6282,.T.);
#5199=FACE_OUTER_BOUND('',#6283,.T.);
#5200=FACE_OUTER_BOUND('',#6284,.T.);
#5201=FACE_OUTER_BOUND('',#6285,.T.);
#5202=FACE_OUTER_BOUND('',#6286,.T.);
#5203=FACE_OUTER_BOUND('',#6287,.T.);
#5204=FACE_OUTER_BOUND('',#6288,.T.);
#5205=FACE_OUTER_BOUND('',#6289,.T.);
#5206=FACE_OUTER_BOUND('',#6290,.T.);
#5207=FACE_OUTER_BOUND('',#6291,.T.);
#5208=FACE_OUTER_BOUND('',#6292,.T.);
#5209=FACE_OUTER_BOUND('',#6293,.T.);
#5210=FACE_OUTER_BOUND('',#6294,.T.);
#5211=FACE_OUTER_BOUND('',#6295,.T.);
#5212=FACE_OUTER_BOUND('',#6296,.T.);
#5213=FACE_OUTER_BOUND('',#6297,.T.);
#5214=FACE_OUTER_BOUND('',#6298,.T.);
#5215=FACE_OUTER_BOUND('',#6299,.T.);
#5216=FACE_OUTER_BOUND('',#6300,.T.);
#5217=FACE_OUTER_BOUND('',#6301,.T.);
#5218=FACE_OUTER_BOUND('',#6302,.T.);
#5219=FACE_OUTER_BOUND('',#6303,.T.);
#5220=FACE_OUTER_BOUND('',#6304,.T.);
#5221=FACE_OUTER_BOUND('',#6305,.T.);
#5222=FACE_OUTER_BOUND('',#6306,.T.);
#5223=FACE_OUTER_BOUND('',#6307,.T.);
#5224=FACE_OUTER_BOUND('',#6308,.T.);
#5225=FACE_OUTER_BOUND('',#6309,.T.);
#5226=FACE_OUTER_BOUND('',#6310,.T.);
#5227=FACE_OUTER_BOUND('',#6311,.T.);
#5228=FACE_OUTER_BOUND('',#6312,.T.);
#5229=FACE_OUTER_BOUND('',#6313,.T.);
#5230=FACE_OUTER_BOUND('',#6314,.T.);
#5231=FACE_OUTER_BOUND('',#6315,.T.);
#5232=FACE_OUTER_BOUND('',#6316,.T.);
#5233=FACE_OUTER_BOUND('',#6317,.T.);
#5234=FACE_OUTER_BOUND('',#6318,.T.);
#5235=FACE_OUTER_BOUND('',#6319,.T.);
#5236=FACE_OUTER_BOUND('',#6320,.T.);
#5237=FACE_OUTER_BOUND('',#6321,.T.);
#5238=FACE_OUTER_BOUND('',#6322,.T.);
#5239=FACE_OUTER_BOUND('',#6323,.T.);
#5240=FACE_OUTER_BOUND('',#6324,.T.);
#5241=FACE_OUTER_BOUND('',#6325,.T.);
#5242=FACE_OUTER_BOUND('',#6326,.T.);
#5243=FACE_OUTER_BOUND('',#6327,.T.);
#5244=FACE_OUTER_BOUND('',#6328,.T.);
#5245=FACE_OUTER_BOUND('',#6329,.T.);
#5246=FACE_OUTER_BOUND('',#6330,.T.);
#5247=FACE_OUTER_BOUND('',#6331,.T.);
#5248=FACE_OUTER_BOUND('',#6332,.T.);
#5249=FACE_OUTER_BOUND('',#6333,.T.);
#5250=FACE_OUTER_BOUND('',#6334,.T.);
#5251=FACE_OUTER_BOUND('',#6335,.T.);
#5252=FACE_OUTER_BOUND('',#6336,.T.);
#5253=FACE_OUTER_BOUND('',#6337,.T.);
#5254=FACE_OUTER_BOUND('',#6338,.T.);
#5255=FACE_OUTER_BOUND('',#6339,.T.);
#5256=FACE_OUTER_BOUND('',#6340,.T.);
#5257=FACE_OUTER_BOUND('',#6341,.T.);
#5258=FACE_OUTER_BOUND('',#6342,.T.);
#5259=FACE_OUTER_BOUND('',#6343,.T.);
#5260=FACE_OUTER_BOUND('',#6344,.T.);
#5261=FACE_OUTER_BOUND('',#6345,.T.);
#5262=FACE_OUTER_BOUND('',#6346,.T.);
#5263=FACE_OUTER_BOUND('',#6347,.T.);
#5264=FACE_OUTER_BOUND('',#6348,.T.);
#5265=FACE_OUTER_BOUND('',#6349,.T.);
#5266=FACE_OUTER_BOUND('',#6350,.T.);
#5267=FACE_OUTER_BOUND('',#6351,.T.);
#5268=FACE_OUTER_BOUND('',#6352,.T.);
#5269=FACE_OUTER_BOUND('',#6353,.T.);
#5270=FACE_OUTER_BOUND('',#6359,.T.);
#5271=FACE_OUTER_BOUND('',#6360,.T.);
#5272=FACE_OUTER_BOUND('',#6366,.T.);
#5273=FACE_OUTER_BOUND('',#6367,.T.);
#5274=FACE_OUTER_BOUND('',#6368,.T.);
#5275=FACE_OUTER_BOUND('',#6369,.T.);
#5276=FACE_OUTER_BOUND('',#6370,.T.);
#5277=FACE_OUTER_BOUND('',#6371,.T.);
#5278=FACE_OUTER_BOUND('',#6372,.T.);
#5279=FACE_OUTER_BOUND('',#6373,.T.);
#5280=FACE_OUTER_BOUND('',#6374,.T.);
#5281=FACE_OUTER_BOUND('',#6375,.T.);
#5282=FACE_OUTER_BOUND('',#6376,.T.);
#5283=FACE_OUTER_BOUND('',#6377,.T.);
#5284=FACE_OUTER_BOUND('',#6378,.T.);
#5285=FACE_OUTER_BOUND('',#6380,.T.);
#5286=FACE_OUTER_BOUND('',#6381,.T.);
#5287=FACE_OUTER_BOUND('',#6382,.T.);
#5288=FACE_OUTER_BOUND('',#6384,.T.);
#5289=FACE_OUTER_BOUND('',#6385,.T.);
#5290=FACE_OUTER_BOUND('',#6386,.T.);
#5291=FACE_OUTER_BOUND('',#6387,.T.);
#5292=FACE_OUTER_BOUND('',#6388,.T.);
#5293=FACE_OUTER_BOUND('',#6390,.T.);
#5294=FACE_OUTER_BOUND('',#6391,.T.);
#5295=FACE_OUTER_BOUND('',#6393,.T.);
#5296=FACE_OUTER_BOUND('',#6394,.T.);
#5297=FACE_OUTER_BOUND('',#6395,.T.);
#5298=FACE_OUTER_BOUND('',#6396,.T.);
#5299=FACE_OUTER_BOUND('',#6397,.T.);
#5300=FACE_OUTER_BOUND('',#6398,.T.);
#5301=FACE_OUTER_BOUND('',#6399,.T.);
#5302=FACE_OUTER_BOUND('',#6400,.T.);
#5303=FACE_OUTER_BOUND('',#6401,.T.);
#5304=FACE_OUTER_BOUND('',#6403,.T.);
#5305=FACE_OUTER_BOUND('',#6404,.T.);
#5306=FACE_OUTER_BOUND('',#6405,.T.);
#5307=FACE_OUTER_BOUND('',#6406,.T.);
#5308=FACE_OUTER_BOUND('',#6407,.T.);
#5309=FACE_OUTER_BOUND('',#6408,.T.);
#5310=FACE_OUTER_BOUND('',#6409,.T.);
#5311=FACE_OUTER_BOUND('',#6410,.T.);
#5312=FACE_OUTER_BOUND('',#6411,.T.);
#5313=FACE_OUTER_BOUND('',#6412,.T.);
#5314=FACE_OUTER_BOUND('',#6413,.T.);
#5315=FACE_OUTER_BOUND('',#6414,.T.);
#5316=FACE_OUTER_BOUND('',#6415,.T.);
#5317=FACE_OUTER_BOUND('',#6416,.T.);
#5318=FACE_OUTER_BOUND('',#6417,.T.);
#5319=FACE_OUTER_BOUND('',#6418,.T.);
#5320=FACE_OUTER_BOUND('',#6419,.T.);
#5321=FACE_OUTER_BOUND('',#6420,.T.);
#5322=FACE_OUTER_BOUND('',#6421,.T.);
#5323=FACE_OUTER_BOUND('',#6422,.T.);
#5324=FACE_OUTER_BOUND('',#6423,.T.);
#5325=FACE_OUTER_BOUND('',#6424,.T.);
#5326=FACE_OUTER_BOUND('',#6425,.T.);
#5327=FACE_OUTER_BOUND('',#6426,.T.);
#5328=FACE_OUTER_BOUND('',#6427,.T.);
#5329=FACE_OUTER_BOUND('',#6428,.T.);
#5330=FACE_OUTER_BOUND('',#6429,.T.);
#5331=FACE_OUTER_BOUND('',#6430,.T.);
#5332=FACE_OUTER_BOUND('',#6431,.T.);
#5333=FACE_OUTER_BOUND('',#6432,.T.);
#5334=FACE_OUTER_BOUND('',#6433,.T.);
#5335=FACE_OUTER_BOUND('',#6434,.T.);
#5336=FACE_OUTER_BOUND('',#6435,.T.);
#5337=FACE_OUTER_BOUND('',#6436,.T.);
#5338=FACE_OUTER_BOUND('',#6437,.T.);
#5339=FACE_OUTER_BOUND('',#6438,.T.);
#5340=FACE_OUTER_BOUND('',#6439,.T.);
#5341=FACE_OUTER_BOUND('',#6440,.T.);
#5342=FACE_OUTER_BOUND('',#6441,.T.);
#5343=FACE_OUTER_BOUND('',#6442,.T.);
#5344=FACE_OUTER_BOUND('',#6443,.T.);
#5345=FACE_OUTER_BOUND('',#6444,.T.);
#5346=FACE_OUTER_BOUND('',#6445,.T.);
#5347=FACE_OUTER_BOUND('',#6446,.T.);
#5348=FACE_OUTER_BOUND('',#6447,.T.);
#5349=FACE_OUTER_BOUND('',#6449,.T.);
#5350=FACE_OUTER_BOUND('',#6451,.T.);
#5351=FACE_OUTER_BOUND('',#6452,.T.);
#5352=FACE_OUTER_BOUND('',#6453,.T.);
#5353=FACE_OUTER_BOUND('',#6454,.T.);
#5354=FACE_OUTER_BOUND('',#6455,.T.);
#5355=FACE_OUTER_BOUND('',#6456,.T.);
#5356=FACE_OUTER_BOUND('',#6457,.T.);
#5357=FACE_OUTER_BOUND('',#6458,.T.);
#5358=FACE_OUTER_BOUND('',#6459,.T.);
#5359=FACE_OUTER_BOUND('',#6460,.T.);
#5360=FACE_OUTER_BOUND('',#6461,.T.);
#5361=FACE_OUTER_BOUND('',#6462,.T.);
#5362=FACE_OUTER_BOUND('',#6463,.T.);
#5363=FACE_OUTER_BOUND('',#6464,.T.);
#5364=FACE_OUTER_BOUND('',#6465,.T.);
#5365=FACE_OUTER_BOUND('',#6466,.T.);
#5366=FACE_OUTER_BOUND('',#6467,.T.);
#5367=FACE_OUTER_BOUND('',#6468,.T.);
#5368=FACE_OUTER_BOUND('',#6469,.T.);
#5369=FACE_OUTER_BOUND('',#6470,.T.);
#5370=FACE_OUTER_BOUND('',#6471,.T.);
#5371=FACE_OUTER_BOUND('',#6472,.T.);
#5372=FACE_OUTER_BOUND('',#6473,.T.);
#5373=FACE_OUTER_BOUND('',#6474,.T.);
#5374=FACE_OUTER_BOUND('',#6475,.T.);
#5375=FACE_OUTER_BOUND('',#6476,.T.);
#5376=FACE_OUTER_BOUND('',#6477,.T.);
#5377=FACE_OUTER_BOUND('',#6478,.T.);
#5378=FACE_OUTER_BOUND('',#6479,.T.);
#5379=FACE_OUTER_BOUND('',#6480,.T.);
#5380=FACE_OUTER_BOUND('',#6481,.T.);
#5381=FACE_OUTER_BOUND('',#6482,.T.);
#5382=FACE_OUTER_BOUND('',#6483,.T.);
#5383=FACE_OUTER_BOUND('',#6484,.T.);
#5384=FACE_OUTER_BOUND('',#6485,.T.);
#5385=FACE_OUTER_BOUND('',#6486,.T.);
#5386=FACE_OUTER_BOUND('',#6487,.T.);
#5387=FACE_OUTER_BOUND('',#6488,.T.);
#5388=FACE_OUTER_BOUND('',#6489,.T.);
#5389=FACE_OUTER_BOUND('',#6490,.T.);
#5390=FACE_OUTER_BOUND('',#6491,.T.);
#5391=FACE_OUTER_BOUND('',#6492,.T.);
#5392=FACE_OUTER_BOUND('',#6493,.T.);
#5393=FACE_OUTER_BOUND('',#6494,.T.);
#5394=FACE_OUTER_BOUND('',#6505,.T.);
#5395=FACE_OUTER_BOUND('',#6516,.T.);
#5396=FACE_OUTER_BOUND('',#6517,.T.);
#5397=FACE_OUTER_BOUND('',#6518,.T.);
#5398=FACE_OUTER_BOUND('',#6519,.T.);
#5399=FACE_OUTER_BOUND('',#6520,.T.);
#5400=FACE_OUTER_BOUND('',#6521,.T.);
#5401=FACE_OUTER_BOUND('',#6522,.T.);
#5402=FACE_OUTER_BOUND('',#6523,.T.);
#5403=FACE_OUTER_BOUND('',#6524,.T.);
#5404=FACE_OUTER_BOUND('',#6525,.T.);
#5405=FACE_OUTER_BOUND('',#6526,.T.);
#5406=FACE_OUTER_BOUND('',#6527,.T.);
#5407=FACE_OUTER_BOUND('',#6528,.T.);
#5408=FACE_OUTER_BOUND('',#6529,.T.);
#5409=FACE_OUTER_BOUND('',#6530,.T.);
#5410=FACE_OUTER_BOUND('',#6531,.T.);
#5411=FACE_OUTER_BOUND('',#6532,.T.);
#5412=FACE_OUTER_BOUND('',#6533,.T.);
#5413=FACE_OUTER_BOUND('',#6534,.T.);
#5414=FACE_OUTER_BOUND('',#6535,.T.);
#5415=FACE_OUTER_BOUND('',#6536,.T.);
#5416=FACE_OUTER_BOUND('',#6537,.T.);
#5417=FACE_OUTER_BOUND('',#6538,.T.);
#5418=FACE_OUTER_BOUND('',#6539,.T.);
#5419=FACE_OUTER_BOUND('',#6540,.T.);
#5420=FACE_OUTER_BOUND('',#6541,.T.);
#5421=FACE_OUTER_BOUND('',#6542,.T.);
#5422=FACE_OUTER_BOUND('',#6543,.T.);
#5423=FACE_OUTER_BOUND('',#6544,.T.);
#5424=FACE_OUTER_BOUND('',#6545,.T.);
#5425=FACE_OUTER_BOUND('',#6546,.T.);
#5426=FACE_OUTER_BOUND('',#6547,.T.);
#5427=FACE_OUTER_BOUND('',#6548,.T.);
#5428=FACE_OUTER_BOUND('',#6549,.T.);
#5429=FACE_OUTER_BOUND('',#6550,.T.);
#5430=FACE_OUTER_BOUND('',#6551,.T.);
#5431=FACE_OUTER_BOUND('',#6552,.T.);
#5432=FACE_OUTER_BOUND('',#6553,.T.);
#5433=FACE_OUTER_BOUND('',#6554,.T.);
#5434=FACE_OUTER_BOUND('',#6555,.T.);
#5435=FACE_OUTER_BOUND('',#6556,.T.);
#5436=FACE_OUTER_BOUND('',#6557,.T.);
#5437=FACE_OUTER_BOUND('',#6558,.T.);
#5438=FACE_OUTER_BOUND('',#6559,.T.);
#5439=FACE_OUTER_BOUND('',#6560,.T.);
#5440=FACE_OUTER_BOUND('',#6561,.T.);
#5441=FACE_OUTER_BOUND('',#6563,.T.);
#5442=FACE_OUTER_BOUND('',#6564,.T.);
#5443=FACE_OUTER_BOUND('',#6565,.T.);
#5444=FACE_OUTER_BOUND('',#6567,.T.);
#5445=FACE_OUTER_BOUND('',#6568,.T.);
#5446=FACE_OUTER_BOUND('',#6569,.T.);
#5447=FACE_OUTER_BOUND('',#6570,.T.);
#5448=FACE_OUTER_BOUND('',#6571,.T.);
#5449=FACE_OUTER_BOUND('',#6572,.T.);
#5450=FACE_OUTER_BOUND('',#6573,.T.);
#5451=FACE_OUTER_BOUND('',#6574,.T.);
#5452=FACE_OUTER_BOUND('',#6575,.T.);
#5453=FACE_OUTER_BOUND('',#6576,.T.);
#5454=FACE_OUTER_BOUND('',#6577,.T.);
#5455=FACE_OUTER_BOUND('',#6578,.T.);
#5456=FACE_OUTER_BOUND('',#6579,.T.);
#5457=FACE_OUTER_BOUND('',#6580,.T.);
#5458=FACE_OUTER_BOUND('',#6581,.T.);
#5459=FACE_OUTER_BOUND('',#6582,.T.);
#5460=FACE_OUTER_BOUND('',#6583,.T.);
#5461=FACE_OUTER_BOUND('',#6584,.T.);
#5462=FACE_OUTER_BOUND('',#6585,.T.);
#5463=FACE_OUTER_BOUND('',#6586,.T.);
#5464=FACE_OUTER_BOUND('',#6587,.T.);
#5465=FACE_OUTER_BOUND('',#6588,.T.);
#5466=FACE_OUTER_BOUND('',#6589,.T.);
#5467=FACE_OUTER_BOUND('',#6590,.T.);
#5468=FACE_OUTER_BOUND('',#6591,.T.);
#5469=FACE_OUTER_BOUND('',#6592,.T.);
#5470=FACE_OUTER_BOUND('',#6593,.T.);
#5471=FACE_OUTER_BOUND('',#6594,.T.);
#5472=FACE_OUTER_BOUND('',#6595,.T.);
#5473=FACE_OUTER_BOUND('',#6596,.T.);
#5474=FACE_OUTER_BOUND('',#6597,.T.);
#5475=FACE_OUTER_BOUND('',#6598,.T.);
#5476=FACE_OUTER_BOUND('',#6599,.T.);
#5477=FACE_OUTER_BOUND('',#6600,.T.);
#5478=FACE_OUTER_BOUND('',#6601,.T.);
#5479=FACE_OUTER_BOUND('',#6602,.T.);
#5480=FACE_OUTER_BOUND('',#6603,.T.);
#5481=FACE_OUTER_BOUND('',#6604,.T.);
#5482=FACE_OUTER_BOUND('',#6605,.T.);
#5483=FACE_OUTER_BOUND('',#6606,.T.);
#5484=FACE_OUTER_BOUND('',#6607,.T.);
#5485=FACE_OUTER_BOUND('',#6608,.T.);
#5486=FACE_OUTER_BOUND('',#6609,.T.);
#5487=FACE_OUTER_BOUND('',#6610,.T.);
#5488=FACE_OUTER_BOUND('',#6611,.T.);
#5489=FACE_OUTER_BOUND('',#6612,.T.);
#5490=FACE_OUTER_BOUND('',#6613,.T.);
#5491=FACE_OUTER_BOUND('',#6614,.T.);
#5492=FACE_OUTER_BOUND('',#6615,.T.);
#5493=FACE_OUTER_BOUND('',#6616,.T.);
#5494=FACE_OUTER_BOUND('',#6617,.T.);
#5495=FACE_OUTER_BOUND('',#6618,.T.);
#5496=FACE_OUTER_BOUND('',#6619,.T.);
#5497=FACE_OUTER_BOUND('',#6620,.T.);
#5498=FACE_OUTER_BOUND('',#6622,.T.);
#5499=FACE_OUTER_BOUND('',#6623,.T.);
#5500=FACE_OUTER_BOUND('',#6624,.T.);
#5501=FACE_OUTER_BOUND('',#6625,.T.);
#5502=FACE_OUTER_BOUND('',#6626,.T.);
#5503=FACE_OUTER_BOUND('',#6627,.T.);
#5504=FACE_OUTER_BOUND('',#6628,.T.);
#5505=FACE_OUTER_BOUND('',#6629,.T.);
#5506=FACE_OUTER_BOUND('',#6630,.T.);
#5507=FACE_OUTER_BOUND('',#6631,.T.);
#5508=FACE_OUTER_BOUND('',#6632,.T.);
#5509=FACE_OUTER_BOUND('',#6633,.T.);
#5510=FACE_OUTER_BOUND('',#6634,.T.);
#5511=FACE_OUTER_BOUND('',#6635,.T.);
#5512=FACE_OUTER_BOUND('',#6636,.T.);
#5513=FACE_OUTER_BOUND('',#6637,.T.);
#5514=FACE_OUTER_BOUND('',#6638,.T.);
#5515=FACE_OUTER_BOUND('',#6639,.T.);
#5516=FACE_OUTER_BOUND('',#6640,.T.);
#5517=FACE_OUTER_BOUND('',#6641,.T.);
#5518=FACE_OUTER_BOUND('',#6642,.T.);
#5519=FACE_OUTER_BOUND('',#6643,.T.);
#5520=FACE_OUTER_BOUND('',#6644,.T.);
#5521=FACE_OUTER_BOUND('',#6645,.T.);
#5522=FACE_OUTER_BOUND('',#6646,.T.);
#5523=FACE_OUTER_BOUND('',#6647,.T.);
#5524=FACE_OUTER_BOUND('',#6648,.T.);
#5525=FACE_OUTER_BOUND('',#6649,.T.);
#5526=FACE_OUTER_BOUND('',#6650,.T.);
#5527=FACE_OUTER_BOUND('',#6651,.T.);
#5528=FACE_OUTER_BOUND('',#6652,.T.);
#5529=FACE_OUTER_BOUND('',#6653,.T.);
#5530=FACE_OUTER_BOUND('',#6654,.T.);
#5531=FACE_OUTER_BOUND('',#6655,.T.);
#5532=FACE_OUTER_BOUND('',#6656,.T.);
#5533=FACE_OUTER_BOUND('',#6657,.T.);
#5534=FACE_OUTER_BOUND('',#6658,.T.);
#5535=FACE_OUTER_BOUND('',#6659,.T.);
#5536=FACE_OUTER_BOUND('',#6660,.T.);
#5537=FACE_OUTER_BOUND('',#6661,.T.);
#5538=FACE_OUTER_BOUND('',#6662,.T.);
#5539=FACE_OUTER_BOUND('',#6663,.T.);
#5540=FACE_OUTER_BOUND('',#6664,.T.);
#5541=FACE_OUTER_BOUND('',#6665,.T.);
#5542=FACE_OUTER_BOUND('',#6666,.T.);
#5543=FACE_OUTER_BOUND('',#6667,.T.);
#5544=FACE_OUTER_BOUND('',#6669,.T.);
#5545=FACE_OUTER_BOUND('',#6670,.T.);
#5546=FACE_OUTER_BOUND('',#6671,.T.);
#5547=FACE_OUTER_BOUND('',#6672,.T.);
#5548=FACE_OUTER_BOUND('',#6673,.T.);
#5549=FACE_OUTER_BOUND('',#6675,.T.);
#5550=FACE_OUTER_BOUND('',#6676,.T.);
#5551=FACE_OUTER_BOUND('',#6678,.T.);
#5552=FACE_OUTER_BOUND('',#6679,.T.);
#5553=FACE_OUTER_BOUND('',#6680,.T.);
#5554=FACE_OUTER_BOUND('',#6681,.T.);
#5555=FACE_OUTER_BOUND('',#6682,.T.);
#5556=FACE_OUTER_BOUND('',#6683,.T.);
#5557=FACE_OUTER_BOUND('',#6684,.T.);
#5558=FACE_OUTER_BOUND('',#6685,.T.);
#5559=FACE_OUTER_BOUND('',#6686,.T.);
#5560=FACE_OUTER_BOUND('',#6687,.T.);
#5561=FACE_OUTER_BOUND('',#6688,.T.);
#5562=FACE_OUTER_BOUND('',#6689,.T.);
#5563=FACE_OUTER_BOUND('',#6690,.T.);
#5564=FACE_OUTER_BOUND('',#6691,.T.);
#5565=FACE_OUTER_BOUND('',#6692,.T.);
#5566=FACE_OUTER_BOUND('',#6693,.T.);
#5567=FACE_OUTER_BOUND('',#6694,.T.);
#5568=FACE_OUTER_BOUND('',#6695,.T.);
#5569=FACE_OUTER_BOUND('',#6696,.T.);
#5570=FACE_OUTER_BOUND('',#6697,.T.);
#5571=FACE_OUTER_BOUND('',#6698,.T.);
#5572=FACE_OUTER_BOUND('',#6699,.T.);
#5573=FACE_OUTER_BOUND('',#6700,.T.);
#5574=FACE_OUTER_BOUND('',#6701,.T.);
#5575=FACE_OUTER_BOUND('',#6702,.T.);
#5576=FACE_OUTER_BOUND('',#6703,.T.);
#5577=FACE_OUTER_BOUND('',#6704,.T.);
#5578=FACE_OUTER_BOUND('',#6705,.T.);
#5579=FACE_OUTER_BOUND('',#6706,.T.);
#5580=FACE_OUTER_BOUND('',#6707,.T.);
#5581=FACE_OUTER_BOUND('',#6708,.T.);
#5582=FACE_OUTER_BOUND('',#6709,.T.);
#5583=FACE_OUTER_BOUND('',#6710,.T.);
#5584=FACE_OUTER_BOUND('',#6711,.T.);
#5585=FACE_OUTER_BOUND('',#6712,.T.);
#5586=FACE_OUTER_BOUND('',#6713,.T.);
#5587=FACE_OUTER_BOUND('',#6714,.T.);
#5588=FACE_OUTER_BOUND('',#6715,.T.);
#5589=FACE_OUTER_BOUND('',#6716,.T.);
#5590=FACE_OUTER_BOUND('',#6717,.T.);
#5591=FACE_OUTER_BOUND('',#6718,.T.);
#5592=FACE_OUTER_BOUND('',#6719,.T.);
#5593=FACE_OUTER_BOUND('',#6720,.T.);
#5594=FACE_OUTER_BOUND('',#6721,.T.);
#5595=FACE_OUTER_BOUND('',#6722,.T.);
#5596=FACE_OUTER_BOUND('',#6723,.T.);
#5597=FACE_OUTER_BOUND('',#6724,.T.);
#5598=FACE_OUTER_BOUND('',#6725,.T.);
#5599=FACE_OUTER_BOUND('',#6726,.T.);
#5600=FACE_OUTER_BOUND('',#6727,.T.);
#5601=FACE_OUTER_BOUND('',#6728,.T.);
#5602=FACE_OUTER_BOUND('',#6729,.T.);
#5603=FACE_OUTER_BOUND('',#6730,.T.);
#5604=FACE_OUTER_BOUND('',#6731,.T.);
#5605=FACE_OUTER_BOUND('',#6732,.T.);
#5606=FACE_OUTER_BOUND('',#6733,.T.);
#5607=FACE_OUTER_BOUND('',#6734,.T.);
#5608=FACE_OUTER_BOUND('',#6735,.T.);
#5609=FACE_OUTER_BOUND('',#6736,.T.);
#5610=FACE_OUTER_BOUND('',#6737,.T.);
#5611=FACE_OUTER_BOUND('',#6738,.T.);
#5612=FACE_OUTER_BOUND('',#6739,.T.);
#5613=FACE_OUTER_BOUND('',#6745,.T.);
#5614=FACE_OUTER_BOUND('',#6746,.T.);
#5615=FACE_OUTER_BOUND('',#6747,.T.);
#5616=FACE_OUTER_BOUND('',#6748,.T.);
#5617=FACE_OUTER_BOUND('',#6749,.T.);
#5618=FACE_OUTER_BOUND('',#6750,.T.);
#5619=FACE_OUTER_BOUND('',#6751,.T.);
#5620=FACE_OUTER_BOUND('',#6752,.T.);
#5621=FACE_OUTER_BOUND('',#6753,.T.);
#5622=FACE_OUTER_BOUND('',#6754,.T.);
#5623=FACE_OUTER_BOUND('',#6755,.T.);
#5624=FACE_OUTER_BOUND('',#6756,.T.);
#5625=FACE_OUTER_BOUND('',#6757,.T.);
#5626=FACE_OUTER_BOUND('',#6758,.T.);
#5627=FACE_OUTER_BOUND('',#6764,.T.);
#5628=FACE_OUTER_BOUND('',#6765,.T.);
#5629=FACE_OUTER_BOUND('',#6766,.T.);
#5630=FACE_OUTER_BOUND('',#6767,.T.);
#5631=FACE_OUTER_BOUND('',#6768,.T.);
#5632=FACE_OUTER_BOUND('',#6769,.T.);
#5633=FACE_OUTER_BOUND('',#6770,.T.);
#5634=FACE_OUTER_BOUND('',#6771,.T.);
#5635=FACE_OUTER_BOUND('',#6772,.T.);
#5636=FACE_OUTER_BOUND('',#6773,.T.);
#5637=FACE_OUTER_BOUND('',#6774,.T.);
#5638=FACE_OUTER_BOUND('',#6775,.T.);
#5639=FACE_OUTER_BOUND('',#6776,.T.);
#5640=FACE_OUTER_BOUND('',#6777,.T.);
#5641=FACE_OUTER_BOUND('',#6778,.T.);
#5642=FACE_OUTER_BOUND('',#6779,.T.);
#5643=FACE_OUTER_BOUND('',#6780,.T.);
#5644=FACE_OUTER_BOUND('',#6781,.T.);
#5645=FACE_OUTER_BOUND('',#6782,.T.);
#5646=FACE_OUTER_BOUND('',#6783,.T.);
#5647=FACE_OUTER_BOUND('',#6784,.T.);
#5648=FACE_OUTER_BOUND('',#6785,.T.);
#5649=FACE_OUTER_BOUND('',#6786,.T.);
#5650=FACE_OUTER_BOUND('',#6787,.T.);
#5651=FACE_OUTER_BOUND('',#6788,.T.);
#5652=FACE_OUTER_BOUND('',#6789,.T.);
#5653=FACE_OUTER_BOUND('',#6790,.T.);
#5654=FACE_OUTER_BOUND('',#6791,.T.);
#5655=FACE_OUTER_BOUND('',#6792,.T.);
#5656=FACE_OUTER_BOUND('',#6793,.T.);
#5657=FACE_OUTER_BOUND('',#6794,.T.);
#5658=FACE_OUTER_BOUND('',#6795,.T.);
#5659=FACE_OUTER_BOUND('',#6796,.T.);
#5660=FACE_OUTER_BOUND('',#6797,.T.);
#5661=FACE_OUTER_BOUND('',#6798,.T.);
#5662=FACE_OUTER_BOUND('',#6799,.T.);
#5663=FACE_OUTER_BOUND('',#6800,.T.);
#5664=FACE_OUTER_BOUND('',#6801,.T.);
#5665=FACE_OUTER_BOUND('',#6802,.T.);
#5666=FACE_OUTER_BOUND('',#6803,.T.);
#5667=FACE_OUTER_BOUND('',#6804,.T.);
#5668=FACE_OUTER_BOUND('',#6805,.T.);
#5669=FACE_OUTER_BOUND('',#6806,.T.);
#5670=FACE_OUTER_BOUND('',#6807,.T.);
#5671=FACE_OUTER_BOUND('',#6808,.T.);
#5672=FACE_OUTER_BOUND('',#6809,.T.);
#5673=FACE_OUTER_BOUND('',#6810,.T.);
#5674=FACE_OUTER_BOUND('',#6811,.T.);
#5675=FACE_OUTER_BOUND('',#6812,.T.);
#5676=FACE_OUTER_BOUND('',#6813,.T.);
#5677=FACE_OUTER_BOUND('',#6814,.T.);
#5678=FACE_OUTER_BOUND('',#6815,.T.);
#5679=FACE_OUTER_BOUND('',#6816,.T.);
#5680=FACE_OUTER_BOUND('',#6817,.T.);
#5681=FACE_OUTER_BOUND('',#6818,.T.);
#5682=FACE_OUTER_BOUND('',#6819,.T.);
#5683=FACE_OUTER_BOUND('',#6820,.T.);
#5684=FACE_OUTER_BOUND('',#6821,.T.);
#5685=FACE_OUTER_BOUND('',#6822,.T.);
#5686=FACE_OUTER_BOUND('',#6823,.T.);
#5687=FACE_OUTER_BOUND('',#6824,.T.);
#5688=FACE_OUTER_BOUND('',#6825,.T.);
#5689=FACE_OUTER_BOUND('',#6826,.T.);
#5690=FACE_OUTER_BOUND('',#6827,.T.);
#5691=FACE_OUTER_BOUND('',#6828,.T.);
#5692=FACE_OUTER_BOUND('',#6829,.T.);
#5693=FACE_OUTER_BOUND('',#6830,.T.);
#5694=FACE_OUTER_BOUND('',#6837,.T.);
#5695=FACE_OUTER_BOUND('',#6838,.T.);
#5696=FACE_OUTER_BOUND('',#6839,.T.);
#5697=FACE_OUTER_BOUND('',#6840,.T.);
#5698=FACE_OUTER_BOUND('',#6841,.T.);
#5699=FACE_OUTER_BOUND('',#6842,.T.);
#5700=FACE_OUTER_BOUND('',#6843,.T.);
#5701=FACE_OUTER_BOUND('',#6844,.T.);
#5702=FACE_OUTER_BOUND('',#6845,.T.);
#5703=FACE_OUTER_BOUND('',#6846,.T.);
#5704=FACE_OUTER_BOUND('',#6847,.T.);
#5705=FACE_OUTER_BOUND('',#6848,.T.);
#5706=FACE_OUTER_BOUND('',#6849,.T.);
#5707=FACE_OUTER_BOUND('',#6850,.T.);
#5708=FACE_OUTER_BOUND('',#6851,.T.);
#5709=FACE_OUTER_BOUND('',#6852,.T.);
#5710=FACE_OUTER_BOUND('',#6853,.T.);
#5711=FACE_OUTER_BOUND('',#6854,.T.);
#5712=FACE_OUTER_BOUND('',#6855,.T.);
#5713=FACE_OUTER_BOUND('',#6856,.T.);
#5714=FACE_OUTER_BOUND('',#6857,.T.);
#5715=FACE_OUTER_BOUND('',#6864,.T.);
#5716=FACE_OUTER_BOUND('',#6865,.T.);
#5717=FACE_OUTER_BOUND('',#6866,.T.);
#5718=FACE_OUTER_BOUND('',#6867,.T.);
#5719=FACE_OUTER_BOUND('',#6868,.T.);
#5720=FACE_OUTER_BOUND('',#6870,.T.);
#5721=FACE_OUTER_BOUND('',#6872,.T.);
#5722=FACE_OUTER_BOUND('',#6873,.T.);
#5723=FACE_OUTER_BOUND('',#6874,.T.);
#5724=FACE_OUTER_BOUND('',#6875,.T.);
#5725=FACE_OUTER_BOUND('',#6876,.T.);
#5726=FACE_OUTER_BOUND('',#6877,.T.);
#5727=FACE_OUTER_BOUND('',#6878,.T.);
#5728=FACE_OUTER_BOUND('',#6879,.T.);
#5729=FACE_OUTER_BOUND('',#6880,.T.);
#5730=FACE_OUTER_BOUND('',#6881,.T.);
#5731=FACE_OUTER_BOUND('',#6882,.T.);
#5732=FACE_OUTER_BOUND('',#6883,.T.);
#5733=FACE_OUTER_BOUND('',#6884,.T.);
#5734=FACE_OUTER_BOUND('',#6885,.T.);
#5735=FACE_OUTER_BOUND('',#6886,.T.);
#5736=FACE_OUTER_BOUND('',#6887,.T.);
#5737=FACE_OUTER_BOUND('',#6888,.T.);
#5738=FACE_OUTER_BOUND('',#6889,.T.);
#5739=FACE_OUTER_BOUND('',#6890,.T.);
#5740=FACE_OUTER_BOUND('',#6891,.T.);
#5741=FACE_OUTER_BOUND('',#6892,.T.);
#5742=FACE_OUTER_BOUND('',#6893,.T.);
#5743=FACE_OUTER_BOUND('',#6894,.T.);
#5744=FACE_OUTER_BOUND('',#6895,.T.);
#5745=FACE_OUTER_BOUND('',#6896,.T.);
#5746=FACE_OUTER_BOUND('',#6897,.T.);
#5747=FACE_OUTER_BOUND('',#6898,.T.);
#5748=FACE_OUTER_BOUND('',#6899,.T.);
#5749=FACE_OUTER_BOUND('',#6900,.T.);
#5750=FACE_OUTER_BOUND('',#6901,.T.);
#5751=FACE_OUTER_BOUND('',#6902,.T.);
#5752=FACE_OUTER_BOUND('',#6903,.T.);
#5753=FACE_OUTER_BOUND('',#6904,.T.);
#5754=FACE_OUTER_BOUND('',#6905,.T.);
#5755=FACE_OUTER_BOUND('',#6906,.T.);
#5756=FACE_OUTER_BOUND('',#6907,.T.);
#5757=FACE_OUTER_BOUND('',#6908,.T.);
#5758=FACE_OUTER_BOUND('',#6909,.T.);
#5759=FACE_OUTER_BOUND('',#6910,.T.);
#5760=FACE_OUTER_BOUND('',#6911,.T.);
#5761=FACE_OUTER_BOUND('',#6912,.T.);
#5762=FACE_OUTER_BOUND('',#6913,.T.);
#5763=FACE_OUTER_BOUND('',#6914,.T.);
#5764=FACE_OUTER_BOUND('',#6915,.T.);
#5765=FACE_OUTER_BOUND('',#6916,.T.);
#5766=FACE_OUTER_BOUND('',#6917,.T.);
#5767=FACE_OUTER_BOUND('',#6918,.T.);
#5768=FACE_OUTER_BOUND('',#6919,.T.);
#5769=FACE_OUTER_BOUND('',#6920,.T.);
#5770=FACE_OUTER_BOUND('',#6921,.T.);
#5771=FACE_OUTER_BOUND('',#6922,.T.);
#5772=FACE_OUTER_BOUND('',#6923,.T.);
#5773=FACE_OUTER_BOUND('',#6924,.T.);
#5774=FACE_OUTER_BOUND('',#6925,.T.);
#5775=FACE_OUTER_BOUND('',#6926,.T.);
#5776=FACE_OUTER_BOUND('',#6927,.T.);
#5777=FACE_OUTER_BOUND('',#6928,.T.);
#5778=FACE_OUTER_BOUND('',#6929,.T.);
#5779=FACE_OUTER_BOUND('',#6930,.T.);
#5780=FACE_OUTER_BOUND('',#6931,.T.);
#5781=FACE_OUTER_BOUND('',#6932,.T.);
#5782=FACE_OUTER_BOUND('',#6933,.T.);
#5783=FACE_OUTER_BOUND('',#6934,.T.);
#5784=FACE_OUTER_BOUND('',#6935,.T.);
#5785=FACE_OUTER_BOUND('',#6936,.T.);
#5786=FACE_OUTER_BOUND('',#6937,.T.);
#5787=FACE_OUTER_BOUND('',#6938,.T.);
#5788=FACE_OUTER_BOUND('',#6939,.T.);
#5789=FACE_OUTER_BOUND('',#6940,.T.);
#5790=FACE_OUTER_BOUND('',#6941,.T.);
#5791=FACE_OUTER_BOUND('',#6942,.T.);
#5792=FACE_OUTER_BOUND('',#6943,.T.);
#5793=FACE_OUTER_BOUND('',#6944,.T.);
#5794=FACE_OUTER_BOUND('',#6945,.T.);
#5795=FACE_OUTER_BOUND('',#6946,.T.);
#5796=FACE_OUTER_BOUND('',#6948,.T.);
#5797=FACE_OUTER_BOUND('',#6949,.T.);
#5798=FACE_OUTER_BOUND('',#6951,.T.);
#5799=FACE_OUTER_BOUND('',#6952,.T.);
#5800=FACE_OUTER_BOUND('',#6953,.T.);
#5801=FACE_OUTER_BOUND('',#6954,.T.);
#5802=FACE_OUTER_BOUND('',#6955,.T.);
#5803=FACE_OUTER_BOUND('',#6956,.T.);
#5804=FACE_OUTER_BOUND('',#6957,.T.);
#5805=FACE_OUTER_BOUND('',#6958,.T.);
#5806=FACE_OUTER_BOUND('',#6959,.T.);
#5807=FACE_OUTER_BOUND('',#6960,.T.);
#5808=FACE_OUTER_BOUND('',#6961,.T.);
#5809=FACE_OUTER_BOUND('',#6962,.T.);
#5810=FACE_OUTER_BOUND('',#6963,.T.);
#5811=FACE_OUTER_BOUND('',#6964,.T.);
#5812=FACE_OUTER_BOUND('',#6965,.T.);
#5813=FACE_OUTER_BOUND('',#6966,.T.);
#5814=FACE_OUTER_BOUND('',#6967,.T.);
#5815=FACE_OUTER_BOUND('',#6968,.T.);
#5816=FACE_OUTER_BOUND('',#6969,.T.);
#5817=FACE_OUTER_BOUND('',#6970,.T.);
#5818=FACE_OUTER_BOUND('',#6971,.T.);
#5819=FACE_OUTER_BOUND('',#6972,.T.);
#5820=FACE_OUTER_BOUND('',#6973,.T.);
#5821=FACE_OUTER_BOUND('',#6975,.T.);
#5822=FACE_OUTER_BOUND('',#6976,.T.);
#5823=FACE_OUTER_BOUND('',#6977,.T.);
#5824=FACE_OUTER_BOUND('',#6978,.T.);
#5825=FACE_OUTER_BOUND('',#6979,.T.);
#5826=FACE_OUTER_BOUND('',#6980,.T.);
#5827=FACE_OUTER_BOUND('',#6981,.T.);
#5828=FACE_OUTER_BOUND('',#6982,.T.);
#5829=FACE_OUTER_BOUND('',#6983,.T.);
#5830=FACE_OUTER_BOUND('',#6984,.T.);
#5831=FACE_OUTER_BOUND('',#6985,.T.);
#5832=FACE_OUTER_BOUND('',#6986,.T.);
#5833=FACE_OUTER_BOUND('',#6987,.T.);
#5834=FACE_OUTER_BOUND('',#6988,.T.);
#5835=FACE_OUTER_BOUND('',#6989,.T.);
#5836=FACE_OUTER_BOUND('',#6990,.T.);
#5837=FACE_OUTER_BOUND('',#6992,.T.);
#5838=EDGE_LOOP('',(#12806,#12807,#12808,#12809,#12810));
#5839=EDGE_LOOP('',(#12811,#12812,#12813,#12814,#12815,#12816));
#5840=EDGE_LOOP('',(#12817));
#5841=EDGE_LOOP('',(#12818));
#5842=EDGE_LOOP('',(#12819,#12820,#12821,#12822,#12823));
#5843=EDGE_LOOP('',(#12824));
#5844=EDGE_LOOP('',(#12825));
#5845=EDGE_LOOP('',(#12826,#12827,#12828,#12829));
#5846=EDGE_LOOP('',(#12830,#12831,#12832,#12833));
#5847=EDGE_LOOP('',(#12834,#12835,#12836,#12837));
#5848=EDGE_LOOP('',(#12838,#12839,#12840,#12841));
#5849=EDGE_LOOP('',(#12842,#12843,#12844,#12845));
#5850=EDGE_LOOP('',(#12846,#12847,#12848,#12849));
#5851=EDGE_LOOP('',(#12850,#12851,#12852,#12853));
#5852=EDGE_LOOP('',(#12854,#12855,#12856,#12857));
#5853=EDGE_LOOP('',(#12858,#12859,#12860,#12861));
#5854=EDGE_LOOP('',(#12862,#12863,#12864,#12865));
#5855=EDGE_LOOP('',(#12866,#12867,#12868,#12869));
#5856=EDGE_LOOP('',(#12870,#12871,#12872,#12873));
#5857=EDGE_LOOP('',(#12874,#12875,#12876,#12877));
#5858=EDGE_LOOP('',(#12878,#12879,#12880,#12881));
#5859=EDGE_LOOP('',(#12882,#12883,#12884,#12885));
#5860=EDGE_LOOP('',(#12886,#12887,#12888,#12889));
#5861=EDGE_LOOP('',(#12890,#12891,#12892,#12893));
#5862=EDGE_LOOP('',(#12894,#12895,#12896,#12897));
#5863=EDGE_LOOP('',(#12898,#12899,#12900,#12901));
#5864=EDGE_LOOP('',(#12902,#12903,#12904,#12905));
#5865=EDGE_LOOP('',(#12906,#12907,#12908,#12909));
#5866=EDGE_LOOP('',(#12910,#12911,#12912,#12913));
#5867=EDGE_LOOP('',(#12914,#12915,#12916,#12917));
#5868=EDGE_LOOP('',(#12918,#12919,#12920,#12921));
#5869=EDGE_LOOP('',(#12922,#12923,#12924,#12925));
#5870=EDGE_LOOP('',(#12926,#12927,#12928,#12929));
#5871=EDGE_LOOP('',(#12930,#12931,#12932,#12933));
#5872=EDGE_LOOP('',(#12934,#12935,#12936,#12937,#12938,#12939,#12940,#12941,
#12942,#12943,#12944,#12945,#12946,#12947,#12948,#12949,#12950,#12951,#12952,
#12953,#12954,#12955,#12956,#12957,#12958,#12959,#12960,#12961,#12962,#12963,
#12964,#12965,#12966,#12967));
#5873=EDGE_LOOP('',(#12968,#12969,#12970,#12971));
#5874=EDGE_LOOP('',(#12972,#12973,#12974,#12975));
#5875=EDGE_LOOP('',(#12976,#12977,#12978,#12979));
#5876=EDGE_LOOP('',(#12980,#12981,#12982,#12983));
#5877=EDGE_LOOP('',(#12984,#12985,#12986,#12987));
#5878=EDGE_LOOP('',(#12988,#12989,#12990,#12991));
#5879=EDGE_LOOP('',(#12992,#12993,#12994,#12995));
#5880=EDGE_LOOP('',(#12996,#12997,#12998,#12999));
#5881=EDGE_LOOP('',(#13000,#13001,#13002,#13003,#13004,#13005,#13006,#13007,
#13008,#13009,#13010,#13011,#13012,#13013,#13014,#13015,#13016,#13017,#13018,
#13019,#13020,#13021,#13022,#13023,#13024,#13025,#13026,#13027,#13028,#13029,
#13030,#13031,#13032,#13033));
#5882=EDGE_LOOP('',(#13034));
#5883=EDGE_LOOP('',(#13035));
#5884=EDGE_LOOP('',(#13036,#13037,#13038,#13039));
#5885=EDGE_LOOP('',(#13040,#13041,#13042,#13043));
#5886=EDGE_LOOP('',(#13044));
#5887=EDGE_LOOP('',(#13045));
#5888=EDGE_LOOP('',(#13046,#13047,#13048,#13049,#13050,#13051,#13052,#13053));
#5889=EDGE_LOOP('',(#13054,#13055,#13056,#13057));
#5890=EDGE_LOOP('',(#13058,#13059,#13060,#13061));
#5891=EDGE_LOOP('',(#13062,#13063,#13064,#13065));
#5892=EDGE_LOOP('',(#13066,#13067,#13068,#13069));
#5893=EDGE_LOOP('',(#13070,#13071,#13072,#13073));
#5894=EDGE_LOOP('',(#13074,#13075,#13076,#13077));
#5895=EDGE_LOOP('',(#13078,#13079,#13080,#13081));
#5896=EDGE_LOOP('',(#13082,#13083,#13084,#13085,#13086,#13087,#13088,#13089));
#5897=EDGE_LOOP('',(#13090,#13091,#13092,#13093));
#5898=EDGE_LOOP('',(#13094,#13095,#13096,#13097));
#5899=EDGE_LOOP('',(#13098,#13099,#13100,#13101));
#5900=EDGE_LOOP('',(#13102,#13103,#13104,#13105));
#5901=EDGE_LOOP('',(#13106,#13107,#13108,#13109));
#5902=EDGE_LOOP('',(#13110,#13111,#13112,#13113));
#5903=EDGE_LOOP('',(#13114,#13115,#13116,#13117,#13118,#13119,#13120,#13121));
#5904=EDGE_LOOP('',(#13122,#13123,#13124,#13125));
#5905=EDGE_LOOP('',(#13126,#13127,#13128,#13129));
#5906=EDGE_LOOP('',(#13130,#13131,#13132,#13133));
#5907=EDGE_LOOP('',(#13134,#13135,#13136,#13137));
#5908=EDGE_LOOP('',(#13138,#13139,#13140,#13141));
#5909=EDGE_LOOP('',(#13142,#13143,#13144,#13145));
#5910=EDGE_LOOP('',(#13146,#13147,#13148,#13149));
#5911=EDGE_LOOP('',(#13150,#13151,#13152,#13153,#13154,#13155,#13156,#13157));
#5912=EDGE_LOOP('',(#13158,#13159,#13160,#13161));
#5913=EDGE_LOOP('',(#13162,#13163,#13164,#13165));
#5914=EDGE_LOOP('',(#13166,#13167,#13168,#13169));
#5915=EDGE_LOOP('',(#13170,#13171,#13172,#13173));
#5916=EDGE_LOOP('',(#13174,#13175,#13176,#13177));
#5917=EDGE_LOOP('',(#13178,#13179,#13180,#13181));
#5918=EDGE_LOOP('',(#13182,#13183,#13184,#13185,#13186,#13187,#13188,#13189));
#5919=EDGE_LOOP('',(#13190,#13191,#13192,#13193));
#5920=EDGE_LOOP('',(#13194,#13195,#13196,#13197));
#5921=EDGE_LOOP('',(#13198,#13199,#13200,#13201));
#5922=EDGE_LOOP('',(#13202,#13203,#13204,#13205));
#5923=EDGE_LOOP('',(#13206,#13207,#13208,#13209));
#5924=EDGE_LOOP('',(#13210,#13211,#13212,#13213));
#5925=EDGE_LOOP('',(#13214,#13215,#13216,#13217));
#5926=EDGE_LOOP('',(#13218,#13219,#13220,#13221,#13222,#13223,#13224,#13225));
#5927=EDGE_LOOP('',(#13226,#13227,#13228,#13229));
#5928=EDGE_LOOP('',(#13230,#13231,#13232,#13233));
#5929=EDGE_LOOP('',(#13234,#13235,#13236,#13237));
#5930=EDGE_LOOP('',(#13238,#13239,#13240,#13241));
#5931=EDGE_LOOP('',(#13242,#13243,#13244,#13245));
#5932=EDGE_LOOP('',(#13246,#13247,#13248,#13249));
#5933=EDGE_LOOP('',(#13250,#13251,#13252,#13253,#13254,#13255,#13256,#13257));
#5934=EDGE_LOOP('',(#13258,#13259,#13260,#13261));
#5935=EDGE_LOOP('',(#13262,#13263,#13264,#13265));
#5936=EDGE_LOOP('',(#13266,#13267,#13268,#13269));
#5937=EDGE_LOOP('',(#13270,#13271,#13272,#13273));
#5938=EDGE_LOOP('',(#13274,#13275,#13276,#13277));
#5939=EDGE_LOOP('',(#13278,#13279,#13280,#13281));
#5940=EDGE_LOOP('',(#13282,#13283,#13284,#13285));
#5941=EDGE_LOOP('',(#13286,#13287,#13288,#13289,#13290,#13291,#13292,#13293));
#5942=EDGE_LOOP('',(#13294,#13295,#13296,#13297));
#5943=EDGE_LOOP('',(#13298,#13299,#13300,#13301));
#5944=EDGE_LOOP('',(#13302,#13303,#13304,#13305));
#5945=EDGE_LOOP('',(#13306,#13307,#13308,#13309));
#5946=EDGE_LOOP('',(#13310,#13311,#13312,#13313));
#5947=EDGE_LOOP('',(#13314,#13315,#13316,#13317));
#5948=EDGE_LOOP('',(#13318,#13319,#13320,#13321,#13322,#13323,#13324,#13325));
#5949=EDGE_LOOP('',(#13326,#13327,#13328,#13329));
#5950=EDGE_LOOP('',(#13330,#13331,#13332,#13333));
#5951=EDGE_LOOP('',(#13334,#13335,#13336,#13337));
#5952=EDGE_LOOP('',(#13338,#13339,#13340,#13341));
#5953=EDGE_LOOP('',(#13342,#13343,#13344,#13345));
#5954=EDGE_LOOP('',(#13346,#13347,#13348,#13349));
#5955=EDGE_LOOP('',(#13350,#13351,#13352,#13353));
#5956=EDGE_LOOP('',(#13354,#13355,#13356,#13357,#13358,#13359,#13360,#13361));
#5957=EDGE_LOOP('',(#13362,#13363,#13364,#13365));
#5958=EDGE_LOOP('',(#13366,#13367,#13368,#13369));
#5959=EDGE_LOOP('',(#13370,#13371,#13372,#13373));
#5960=EDGE_LOOP('',(#13374,#13375,#13376,#13377));
#5961=EDGE_LOOP('',(#13378,#13379,#13380,#13381));
#5962=EDGE_LOOP('',(#13382,#13383,#13384,#13385));
#5963=EDGE_LOOP('',(#13386,#13387,#13388,#13389,#13390,#13391,#13392,#13393));
#5964=EDGE_LOOP('',(#13394,#13395,#13396,#13397));
#5965=EDGE_LOOP('',(#13398,#13399,#13400,#13401));
#5966=EDGE_LOOP('',(#13402,#13403,#13404,#13405));
#5967=EDGE_LOOP('',(#13406,#13407,#13408,#13409));
#5968=EDGE_LOOP('',(#13410,#13411,#13412,#13413));
#5969=EDGE_LOOP('',(#13414,#13415,#13416,#13417));
#5970=EDGE_LOOP('',(#13418,#13419,#13420,#13421));
#5971=EDGE_LOOP('',(#13422,#13423,#13424,#13425,#13426,#13427,#13428,#13429));
#5972=EDGE_LOOP('',(#13430,#13431,#13432,#13433));
#5973=EDGE_LOOP('',(#13434,#13435,#13436,#13437));
#5974=EDGE_LOOP('',(#13438,#13439,#13440,#13441));
#5975=EDGE_LOOP('',(#13442,#13443,#13444,#13445));
#5976=EDGE_LOOP('',(#13446,#13447,#13448,#13449));
#5977=EDGE_LOOP('',(#13450,#13451,#13452,#13453));
#5978=EDGE_LOOP('',(#13454,#13455,#13456,#13457,#13458,#13459,#13460,#13461));
#5979=EDGE_LOOP('',(#13462,#13463,#13464,#13465));
#5980=EDGE_LOOP('',(#13466,#13467,#13468,#13469));
#5981=EDGE_LOOP('',(#13470,#13471,#13472,#13473));
#5982=EDGE_LOOP('',(#13474,#13475,#13476,#13477));
#5983=EDGE_LOOP('',(#13478,#13479,#13480,#13481));
#5984=EDGE_LOOP('',(#13482,#13483,#13484,#13485));
#5985=EDGE_LOOP('',(#13486,#13487,#13488,#13489));
#5986=EDGE_LOOP('',(#13490,#13491,#13492,#13493,#13494,#13495,#13496,#13497));
#5987=EDGE_LOOP('',(#13498,#13499,#13500,#13501));
#5988=EDGE_LOOP('',(#13502,#13503,#13504,#13505));
#5989=EDGE_LOOP('',(#13506,#13507,#13508,#13509));
#5990=EDGE_LOOP('',(#13510,#13511,#13512,#13513));
#5991=EDGE_LOOP('',(#13514,#13515,#13516,#13517));
#5992=EDGE_LOOP('',(#13518,#13519,#13520,#13521));
#5993=EDGE_LOOP('',(#13522,#13523,#13524,#13525,#13526,#13527,#13528,#13529));
#5994=EDGE_LOOP('',(#13530,#13531,#13532,#13533));
#5995=EDGE_LOOP('',(#13534,#13535,#13536,#13537));
#5996=EDGE_LOOP('',(#13538,#13539,#13540,#13541));
#5997=EDGE_LOOP('',(#13542,#13543,#13544,#13545));
#5998=EDGE_LOOP('',(#13546,#13547,#13548,#13549));
#5999=EDGE_LOOP('',(#13550,#13551,#13552,#13553));
#6000=EDGE_LOOP('',(#13554,#13555,#13556,#13557));
#6001=EDGE_LOOP('',(#13558,#13559,#13560,#13561,#13562,#13563,#13564,#13565));
#6002=EDGE_LOOP('',(#13566,#13567,#13568,#13569));
#6003=EDGE_LOOP('',(#13570,#13571,#13572,#13573));
#6004=EDGE_LOOP('',(#13574,#13575,#13576,#13577));
#6005=EDGE_LOOP('',(#13578,#13579,#13580,#13581));
#6006=EDGE_LOOP('',(#13582,#13583,#13584,#13585,#13586,#13587));
#6007=EDGE_LOOP('',(#13588,#13589,#13590,#13591));
#6008=EDGE_LOOP('',(#13592,#13593,#13594,#13595,#13596,#13597,#13598,#13599));
#6009=EDGE_LOOP('',(#13600,#13601,#13602,#13603,#13604,#13605,#13606,#13607));
#6010=EDGE_LOOP('',(#13608,#13609,#13610,#13611));
#6011=EDGE_LOOP('',(#13612,#13613,#13614,#13615));
#6012=EDGE_LOOP('',(#13616,#13617,#13618,#13619,#13620));
#6013=EDGE_LOOP('',(#13621,#13622,#13623,#13624,#13625));
#6014=EDGE_LOOP('',(#13626,#13627,#13628,#13629));
#6015=EDGE_LOOP('',(#13630,#13631,#13632,#13633));
#6016=EDGE_LOOP('',(#13634,#13635,#13636,#13637));
#6017=EDGE_LOOP('',(#13638,#13639,#13640,#13641,#13642,#13643,#13644,#13645,
#13646,#13647));
#6018=EDGE_LOOP('',(#13648,#13649,#13650,#13651,#13652,#13653,#13654,#13655,
#13656,#13657,#13658,#13659));
#6019=EDGE_LOOP('',(#13660,#13661,#13662,#13663));
#6020=EDGE_LOOP('',(#13664,#13665,#13666,#13667));
#6021=EDGE_LOOP('',(#13668,#13669,#13670,#13671));
#6022=EDGE_LOOP('',(#13672,#13673,#13674,#13675));
#6023=EDGE_LOOP('',(#13676,#13677,#13678,#13679));
#6024=EDGE_LOOP('',(#13680,#13681,#13682,#13683));
#6025=EDGE_LOOP('',(#13684,#13685,#13686,#13687));
#6026=EDGE_LOOP('',(#13688,#13689,#13690,#13691));
#6027=EDGE_LOOP('',(#13692,#13693,#13694,#13695));
#6028=EDGE_LOOP('',(#13696,#13697,#13698,#13699));
#6029=EDGE_LOOP('',(#13700,#13701,#13702,#13703));
#6030=EDGE_LOOP('',(#13704,#13705,#13706,#13707));
#6031=EDGE_LOOP('',(#13708,#13709,#13710,#13711));
#6032=EDGE_LOOP('',(#13712,#13713,#13714,#13715));
#6033=EDGE_LOOP('',(#13716,#13717,#13718,#13719,#13720,#13721));
#6034=EDGE_LOOP('',(#13722,#13723,#13724,#13725,#13726,#13727,#13728));
#6035=EDGE_LOOP('',(#13729,#13730,#13731,#13732,#13733,#13734,#13735));
#6036=EDGE_LOOP('',(#13736,#13737));
#6037=EDGE_LOOP('',(#13738,#13739,#13740,#13741,#13742,#13743,#13744,#13745));
#6038=EDGE_LOOP('',(#13746,#13747,#13748,#13749));
#6039=EDGE_LOOP('',(#13750,#13751,#13752,#13753));
#6040=EDGE_LOOP('',(#13754,#13755,#13756,#13757));
#6041=EDGE_LOOP('',(#13758,#13759,#13760,#13761));
#6042=EDGE_LOOP('',(#13762,#13763,#13764,#13765,#13766,#13767,#13768,#13769,
#13770,#13771,#13772,#13773,#13774,#13775));
#6043=EDGE_LOOP('',(#13776,#13777,#13778,#13779,#13780,#13781));
#6044=EDGE_LOOP('',(#13782,#13783,#13784,#13785));
#6045=EDGE_LOOP('',(#13786,#13787,#13788,#13789));
#6046=EDGE_LOOP('',(#13790,#13791,#13792,#13793));
#6047=EDGE_LOOP('',(#13794,#13795,#13796,#13797));
#6048=EDGE_LOOP('',(#13798,#13799,#13800,#13801));
#6049=EDGE_LOOP('',(#13802,#13803,#13804,#13805));
#6050=EDGE_LOOP('',(#13806,#13807,#13808,#13809));
#6051=EDGE_LOOP('',(#13810,#13811,#13812,#13813));
#6052=EDGE_LOOP('',(#13814,#13815,#13816,#13817));
#6053=EDGE_LOOP('',(#13818,#13819,#13820,#13821));
#6054=EDGE_LOOP('',(#13822,#13823,#13824,#13825));
#6055=EDGE_LOOP('',(#13826,#13827,#13828,#13829));
#6056=EDGE_LOOP('',(#13830,#13831,#13832,#13833));
#6057=EDGE_LOOP('',(#13834,#13835,#13836,#13837));
#6058=EDGE_LOOP('',(#13838,#13839,#13840,#13841));
#6059=EDGE_LOOP('',(#13842,#13843,#13844,#13845));
#6060=EDGE_LOOP('',(#13846,#13847,#13848,#13849));
#6061=EDGE_LOOP('',(#13850,#13851,#13852,#13853));
#6062=EDGE_LOOP('',(#13854,#13855,#13856,#13857));
#6063=EDGE_LOOP('',(#13858,#13859,#13860,#13861));
#6064=EDGE_LOOP('',(#13862,#13863,#13864,#13865));
#6065=EDGE_LOOP('',(#13866,#13867,#13868,#13869));
#6066=EDGE_LOOP('',(#13870,#13871,#13872,#13873));
#6067=EDGE_LOOP('',(#13874,#13875,#13876,#13877));
#6068=EDGE_LOOP('',(#13878,#13879,#13880,#13881));
#6069=EDGE_LOOP('',(#13882,#13883,#13884,#13885));
#6070=EDGE_LOOP('',(#13886,#13887,#13888,#13889));
#6071=EDGE_LOOP('',(#13890,#13891,#13892,#13893));
#6072=EDGE_LOOP('',(#13894,#13895,#13896,#13897));
#6073=EDGE_LOOP('',(#13898,#13899,#13900,#13901));
#6074=EDGE_LOOP('',(#13902,#13903,#13904,#13905));
#6075=EDGE_LOOP('',(#13906,#13907,#13908,#13909));
#6076=EDGE_LOOP('',(#13910,#13911,#13912,#13913));
#6077=EDGE_LOOP('',(#13914,#13915,#13916,#13917));
#6078=EDGE_LOOP('',(#13918,#13919,#13920,#13921));
#6079=EDGE_LOOP('',(#13922,#13923,#13924,#13925));
#6080=EDGE_LOOP('',(#13926,#13927,#13928,#13929));
#6081=EDGE_LOOP('',(#13930,#13931,#13932,#13933));
#6082=EDGE_LOOP('',(#13934,#13935,#13936,#13937));
#6083=EDGE_LOOP('',(#13938,#13939,#13940,#13941));
#6084=EDGE_LOOP('',(#13942,#13943,#13944,#13945));
#6085=EDGE_LOOP('',(#13946,#13947,#13948,#13949));
#6086=EDGE_LOOP('',(#13950,#13951,#13952,#13953));
#6087=EDGE_LOOP('',(#13954,#13955,#13956,#13957));
#6088=EDGE_LOOP('',(#13958,#13959,#13960,#13961));
#6089=EDGE_LOOP('',(#13962,#13963,#13964,#13965));
#6090=EDGE_LOOP('',(#13966,#13967,#13968,#13969,#13970,#13971,#13972,#13973,
#13974,#13975,#13976,#13977,#13978,#13979,#13980,#13981,#13982,#13983,#13984,
#13985,#13986,#13987,#13988,#13989,#13990,#13991,#13992,#13993,#13994,#13995,
#13996,#13997,#13998,#13999,#14000,#14001,#14002,#14003,#14004,#14005,#14006,
#14007,#14008,#14009,#14010,#14011,#14012,#14013,#14014,#14015,#14016,#14017,
#14018,#14019,#14020,#14021,#14022,#14023,#14024,#14025,#14026,#14027,#14028,
#14029,#14030,#14031,#14032,#14033,#14034,#14035,#14036,#14037,#14038,#14039,
#14040,#14041,#14042,#14043,#14044,#14045,#14046,#14047,#14048,#14049,#14050,
#14051,#14052,#14053,#14054,#14055));
#6091=EDGE_LOOP('',(#14056));
#6092=EDGE_LOOP('',(#14057,#14058,#14059,#14060));
#6093=EDGE_LOOP('',(#14061,#14062,#14063,#14064));
#6094=EDGE_LOOP('',(#14065,#14066,#14067,#14068));
#6095=EDGE_LOOP('',(#14069,#14070,#14071,#14072));
#6096=EDGE_LOOP('',(#14073,#14074,#14075,#14076));
#6097=EDGE_LOOP('',(#14077,#14078,#14079,#14080));
#6098=EDGE_LOOP('',(#14081,#14082,#14083,#14084));
#6099=EDGE_LOOP('',(#14085,#14086,#14087,#14088));
#6100=EDGE_LOOP('',(#14089,#14090,#14091,#14092));
#6101=EDGE_LOOP('',(#14093,#14094,#14095,#14096));
#6102=EDGE_LOOP('',(#14097,#14098,#14099,#14100));
#6103=EDGE_LOOP('',(#14101,#14102,#14103,#14104));
#6104=EDGE_LOOP('',(#14105,#14106,#14107,#14108));
#6105=EDGE_LOOP('',(#14109,#14110,#14111,#14112));
#6106=EDGE_LOOP('',(#14113,#14114,#14115,#14116));
#6107=EDGE_LOOP('',(#14117,#14118,#14119,#14120));
#6108=EDGE_LOOP('',(#14121,#14122,#14123,#14124));
#6109=EDGE_LOOP('',(#14125,#14126,#14127,#14128));
#6110=EDGE_LOOP('',(#14129,#14130,#14131,#14132));
#6111=EDGE_LOOP('',(#14133,#14134,#14135,#14136));
#6112=EDGE_LOOP('',(#14137,#14138,#14139,#14140));
#6113=EDGE_LOOP('',(#14141,#14142,#14143,#14144));
#6114=EDGE_LOOP('',(#14145,#14146,#14147,#14148));
#6115=EDGE_LOOP('',(#14149,#14150,#14151,#14152));
#6116=EDGE_LOOP('',(#14153,#14154,#14155,#14156));
#6117=EDGE_LOOP('',(#14157,#14158,#14159,#14160));
#6118=EDGE_LOOP('',(#14161,#14162,#14163,#14164));
#6119=EDGE_LOOP('',(#14165,#14166,#14167,#14168));
#6120=EDGE_LOOP('',(#14169,#14170,#14171,#14172));
#6121=EDGE_LOOP('',(#14173,#14174,#14175,#14176));
#6122=EDGE_LOOP('',(#14177,#14178,#14179,#14180));
#6123=EDGE_LOOP('',(#14181,#14182,#14183,#14184));
#6124=EDGE_LOOP('',(#14185,#14186,#14187,#14188));
#6125=EDGE_LOOP('',(#14189,#14190,#14191,#14192));
#6126=EDGE_LOOP('',(#14193,#14194,#14195,#14196));
#6127=EDGE_LOOP('',(#14197,#14198,#14199,#14200));
#6128=EDGE_LOOP('',(#14201,#14202,#14203,#14204));
#6129=EDGE_LOOP('',(#14205,#14206,#14207,#14208));
#6130=EDGE_LOOP('',(#14209,#14210,#14211,#14212));
#6131=EDGE_LOOP('',(#14213,#14214,#14215,#14216));
#6132=EDGE_LOOP('',(#14217,#14218,#14219,#14220));
#6133=EDGE_LOOP('',(#14221,#14222,#14223,#14224));
#6134=EDGE_LOOP('',(#14225,#14226,#14227,#14228));
#6135=EDGE_LOOP('',(#14229,#14230,#14231,#14232));
#6136=EDGE_LOOP('',(#14233,#14234,#14235,#14236));
#6137=EDGE_LOOP('',(#14237,#14238,#14239,#14240,#14241,#14242,#14243,#14244,
#14245,#14246,#14247,#14248,#14249,#14250,#14251,#14252,#14253,#14254,#14255,
#14256,#14257,#14258,#14259,#14260,#14261,#14262,#14263,#14264,#14265,#14266,
#14267,#14268,#14269,#14270,#14271,#14272,#14273,#14274,#14275,#14276,#14277,
#14278,#14279,#14280,#14281,#14282,#14283,#14284,#14285,#14286,#14287,#14288,
#14289,#14290,#14291,#14292,#14293,#14294,#14295,#14296,#14297,#14298,#14299,
#14300,#14301,#14302,#14303,#14304,#14305,#14306,#14307,#14308,#14309,#14310,
#14311,#14312,#14313,#14314,#14315,#14316,#14317,#14318,#14319,#14320,#14321,
#14322,#14323,#14324,#14325,#14326));
#6138=EDGE_LOOP('',(#14327));
#6139=EDGE_LOOP('',(#14328,#14329,#14330,#14331));
#6140=EDGE_LOOP('',(#14332,#14333,#14334,#14335));
#6141=EDGE_LOOP('',(#14336,#14337,#14338,#14339));
#6142=EDGE_LOOP('',(#14340,#14341,#14342,#14343,#14344));
#6143=EDGE_LOOP('',(#14345,#14346,#14347,#14348,#14349,#14350,#14351,#14352));
#6144=EDGE_LOOP('',(#14353,#14354,#14355,#14356,#14357));
#6145=EDGE_LOOP('',(#14358,#14359,#14360,#14361));
#6146=EDGE_LOOP('',(#14362,#14363,#14364,#14365,#14366));
#6147=EDGE_LOOP('',(#14367,#14368,#14369,#14370,#14371,#14372,#14373,#14374));
#6148=EDGE_LOOP('',(#14375,#14376,#14377,#14378,#14379));
#6149=EDGE_LOOP('',(#14380,#14381,#14382,#14383));
#6150=EDGE_LOOP('',(#14384,#14385,#14386,#14387,#14388));
#6151=EDGE_LOOP('',(#14389,#14390,#14391,#14392,#14393,#14394,#14395,#14396));
#6152=EDGE_LOOP('',(#14397,#14398,#14399,#14400));
#6153=EDGE_LOOP('',(#14401,#14402,#14403,#14404));
#6154=EDGE_LOOP('',(#14405,#14406,#14407,#14408,#14409));
#6155=EDGE_LOOP('',(#14410,#14411,#14412,#14413));
#6156=EDGE_LOOP('',(#14414,#14415,#14416,#14417,#14418));
#6157=EDGE_LOOP('',(#14419,#14420,#14421,#14422,#14423,#14424,#14425,#14426));
#6158=EDGE_LOOP('',(#14427,#14428,#14429,#14430,#14431));
#6159=EDGE_LOOP('',(#14432,#14433,#14434,#14435,#14436));
#6160=EDGE_LOOP('',(#14437,#14438,#14439,#14440));
#6161=EDGE_LOOP('',(#14441,#14442,#14443,#14444,#14445));
#6162=EDGE_LOOP('',(#14446,#14447,#14448,#14449));
#6163=EDGE_LOOP('',(#14450,#14451,#14452,#14453,#14454,#14455,#14456));
#6164=EDGE_LOOP('',(#14457,#14458,#14459,#14460));
#6165=EDGE_LOOP('',(#14461,#14462,#14463,#14464,#14465,#14466));
#6166=EDGE_LOOP('',(#14467,#14468,#14469,#14470,#14471,#14472,#14473));
#6167=EDGE_LOOP('',(#14474,#14475,#14476,#14477));
#6168=EDGE_LOOP('',(#14478,#14479,#14480,#14481,#14482,#14483));
#6169=EDGE_LOOP('',(#14484,#14485,#14486,#14487,#14488,#14489,#14490));
#6170=EDGE_LOOP('',(#14491,#14492,#14493,#14494,#14495));
#6171=EDGE_LOOP('',(#14496,#14497,#14498,#14499));
#6172=EDGE_LOOP('',(#14500,#14501,#14502,#14503,#14504,#14505,#14506));
#6173=EDGE_LOOP('',(#14507,#14508,#14509,#14510));
#6174=EDGE_LOOP('',(#14511,#14512,#14513,#14514,#14515,#14516,#14517,#14518,
#14519,#14520,#14521,#14522,#14523,#14524,#14525,#14526,#14527,#14528,#14529,
#14530,#14531,#14532,#14533,#14534));
#6175=EDGE_LOOP('',(#14535));
#6176=EDGE_LOOP('',(#14536,#14537,#14538,#14539,#14540));
#6177=EDGE_LOOP('',(#14541,#14542,#14543,#14544,#14545));
#6178=EDGE_LOOP('',(#14546,#14547,#14548,#14549,#14550,#14551,#14552));
#6179=EDGE_LOOP('',(#14553,#14554,#14555,#14556,#14557));
#6180=EDGE_LOOP('',(#14558,#14559,#14560,#14561,#14562));
#6181=EDGE_LOOP('',(#14563,#14564,#14565,#14566));
#6182=EDGE_LOOP('',(#14567,#14568,#14569,#14570,#14571));
#6183=EDGE_LOOP('',(#14572,#14573,#14574,#14575,#14576,#14577,#14578,#14579,
#14580,#14581,#14582,#14583,#14584,#14585,#14586,#14587,#14588,#14589,#14590,
#14591,#14592,#14593,#14594,#14595,#14596,#14597,#14598,#14599));
#6184=EDGE_LOOP('',(#14600));
#6185=EDGE_LOOP('',(#14601));
#6186=EDGE_LOOP('',(#14602));
#6187=EDGE_LOOP('',(#14603));
#6188=EDGE_LOOP('',(#14604,#14605,#14606,#14607));
#6189=EDGE_LOOP('',(#14608,#14609,#14610,#14611,#14612,#14613,#14614,#14615));
#6190=EDGE_LOOP('',(#14616,#14617,#14618,#14619,#14620));
#6191=EDGE_LOOP('',(#14621,#14622,#14623,#14624));
#6192=EDGE_LOOP('',(#14625,#14626,#14627,#14628));
#6193=EDGE_LOOP('',(#14629,#14630,#14631,#14632));
#6194=EDGE_LOOP('',(#14633,#14634,#14635,#14636));
#6195=EDGE_LOOP('',(#14637,#14638,#14639,#14640,#14641,#14642,#14643));
#6196=EDGE_LOOP('',(#14644,#14645,#14646,#14647));
#6197=EDGE_LOOP('',(#14648,#14649,#14650,#14651));
#6198=EDGE_LOOP('',(#14652,#14653,#14654,#14655));
#6199=EDGE_LOOP('',(#14656,#14657,#14658,#14659));
#6200=EDGE_LOOP('',(#14660,#14661,#14662,#14663));
#6201=EDGE_LOOP('',(#14664,#14665,#14666,#14667));
#6202=EDGE_LOOP('',(#14668,#14669,#14670,#14671));
#6203=EDGE_LOOP('',(#14672,#14673,#14674,#14675,#14676,#14677,#14678,#14679));
#6204=EDGE_LOOP('',(#14680,#14681,#14682,#14683));
#6205=EDGE_LOOP('',(#14684,#14685,#14686,#14687,#14688,#14689));
#6206=EDGE_LOOP('',(#14690,#14691,#14692,#14693,#14694));
#6207=EDGE_LOOP('',(#14695,#14696,#14697,#14698));
#6208=EDGE_LOOP('',(#14699,#14700,#14701,#14702));
#6209=EDGE_LOOP('',(#14703,#14704,#14705,#14706));
#6210=EDGE_LOOP('',(#14707,#14708,#14709,#14710));
#6211=EDGE_LOOP('',(#14711,#14712));
#6212=EDGE_LOOP('',(#14713,#14714,#14715,#14716));
#6213=EDGE_LOOP('',(#14717,#14718));
#6214=EDGE_LOOP('',(#14719,#14720,#14721,#14722));
#6215=EDGE_LOOP('',(#14723,#14724));
#6216=EDGE_LOOP('',(#14725,#14726,#14727,#14728,#14729,#14730,#14731,#14732));
#6217=EDGE_LOOP('',(#14733,#14734,#14735,#14736,#14737,#14738,#14739,#14740));
#6218=EDGE_LOOP('',(#14741,#14742,#14743,#14744));
#6219=EDGE_LOOP('',(#14745,#14746));
#6220=EDGE_LOOP('',(#14747,#14748,#14749,#14750,#14751,#14752,#14753,#14754));
#6221=EDGE_LOOP('',(#14755,#14756,#14757,#14758,#14759,#14760));
#6222=EDGE_LOOP('',(#14761,#14762,#14763,#14764));
#6223=EDGE_LOOP('',(#14765));
#6224=EDGE_LOOP('',(#14766));
#6225=EDGE_LOOP('',(#14767,#14768,#14769,#14770));
#6226=EDGE_LOOP('',(#14771,#14772,#14773,#14774,#14775));
#6227=EDGE_LOOP('',(#14776,#14777,#14778,#14779,#14780));
#6228=EDGE_LOOP('',(#14781));
#6229=EDGE_LOOP('',(#14782));
#6230=EDGE_LOOP('',(#14783,#14784,#14785,#14786));
#6231=EDGE_LOOP('',(#14787));
#6232=EDGE_LOOP('',(#14788));
#6233=EDGE_LOOP('',(#14789,#14790,#14791,#14792));
#6234=EDGE_LOOP('',(#14793));
#6235=EDGE_LOOP('',(#14794));
#6236=EDGE_LOOP('',(#14795,#14796,#14797,#14798));
#6237=EDGE_LOOP('',(#14799));
#6238=EDGE_LOOP('',(#14800));
#6239=EDGE_LOOP('',(#14801,#14802,#14803,#14804));
#6240=EDGE_LOOP('',(#14805,#14806,#14807,#14808,#14809,#14810,#14811,#14812,
#14813,#14814,#14815,#14816,#14817,#14818,#14819,#14820,#14821,#14822,#14823,
#14824,#14825,#14826,#14827,#14828,#14829,#14830,#14831,#14832));
#6241=EDGE_LOOP('',(#14833,#14834,#14835,#14836,#14837,#14838,#14839,#14840));
#6242=EDGE_LOOP('',(#14841));
#6243=EDGE_LOOP('',(#14842,#14843,#14844,#14845));
#6244=EDGE_LOOP('',(#14846));
#6245=EDGE_LOOP('',(#14847));
#6246=EDGE_LOOP('',(#14848));
#6247=EDGE_LOOP('',(#14849));
#6248=EDGE_LOOP('',(#14850,#14851,#14852,#14853));
#6249=EDGE_LOOP('',(#14854,#14855,#14856,#14857));
#6250=EDGE_LOOP('',(#14858,#14859,#14860,#14861));
#6251=EDGE_LOOP('',(#14862,#14863,#14864,#14865,#14866,#14867));
#6252=EDGE_LOOP('',(#14868,#14869,#14870,#14871,#14872));
#6253=EDGE_LOOP('',(#14873,#14874,#14875,#14876,#14877,#14878));
#6254=EDGE_LOOP('',(#14879));
#6255=EDGE_LOOP('',(#14880));
#6256=EDGE_LOOP('',(#14881,#14882,#14883,#14884,#14885));
#6257=EDGE_LOOP('',(#14886));
#6258=EDGE_LOOP('',(#14887));
#6259=EDGE_LOOP('',(#14888,#14889,#14890,#14891));
#6260=EDGE_LOOP('',(#14892,#14893,#14894,#14895));
#6261=EDGE_LOOP('',(#14896,#14897,#14898,#14899));
#6262=EDGE_LOOP('',(#14900,#14901,#14902,#14903));
#6263=EDGE_LOOP('',(#14904,#14905,#14906,#14907));
#6264=EDGE_LOOP('',(#14908,#14909,#14910,#14911,#14912,#14913,#14914));
#6265=EDGE_LOOP('',(#14915,#14916,#14917,#14918));
#6266=EDGE_LOOP('',(#14919,#14920,#14921,#14922,#14923,#14924,#14925));
#6267=EDGE_LOOP('',(#14926,#14927,#14928,#14929));
#6268=EDGE_LOOP('',(#14930,#14931,#14932,#14933));
#6269=EDGE_LOOP('',(#14934,#14935,#14936,#14937));
#6270=EDGE_LOOP('',(#14938,#14939,#14940,#14941,#14942,#14943,#14944));
#6271=EDGE_LOOP('',(#14945,#14946,#14947,#14948));
#6272=EDGE_LOOP('',(#14949,#14950,#14951,#14952,#14953,#14954,#14955));
#6273=EDGE_LOOP('',(#14956,#14957,#14958,#14959));
#6274=EDGE_LOOP('',(#14960,#14961,#14962,#14963));
#6275=EDGE_LOOP('',(#14964,#14965,#14966,#14967));
#6276=EDGE_LOOP('',(#14968,#14969,#14970,#14971));
#6277=EDGE_LOOP('',(#14972,#14973,#14974,#14975));
#6278=EDGE_LOOP('',(#14976,#14977,#14978,#14979));
#6279=EDGE_LOOP('',(#14980,#14981,#14982,#14983));
#6280=EDGE_LOOP('',(#14984,#14985,#14986,#14987));
#6281=EDGE_LOOP('',(#14988,#14989,#14990,#14991));
#6282=EDGE_LOOP('',(#14992,#14993,#14994,#14995));
#6283=EDGE_LOOP('',(#14996,#14997,#14998,#14999));
#6284=EDGE_LOOP('',(#15000,#15001,#15002,#15003));
#6285=EDGE_LOOP('',(#15004,#15005,#15006,#15007));
#6286=EDGE_LOOP('',(#15008,#15009,#15010,#15011));
#6287=EDGE_LOOP('',(#15012,#15013,#15014,#15015));
#6288=EDGE_LOOP('',(#15016,#15017,#15018,#15019));
#6289=EDGE_LOOP('',(#15020,#15021,#15022,#15023));
#6290=EDGE_LOOP('',(#15024,#15025,#15026,#15027));
#6291=EDGE_LOOP('',(#15028,#15029,#15030,#15031));
#6292=EDGE_LOOP('',(#15032,#15033,#15034,#15035));
#6293=EDGE_LOOP('',(#15036,#15037,#15038,#15039));
#6294=EDGE_LOOP('',(#15040,#15041,#15042,#15043));
#6295=EDGE_LOOP('',(#15044,#15045,#15046,#15047));
#6296=EDGE_LOOP('',(#15048,#15049,#15050,#15051));
#6297=EDGE_LOOP('',(#15052,#15053,#15054,#15055));
#6298=EDGE_LOOP('',(#15056,#15057,#15058,#15059,#15060,#15061,#15062,#15063,
#15064,#15065,#15066,#15067,#15068,#15069,#15070,#15071,#15072,#15073,#15074,
#15075));
#6299=EDGE_LOOP('',(#15076,#15077,#15078,#15079,#15080,#15081,#15082,#15083,
#15084,#15085,#15086,#15087,#15088,#15089,#15090,#15091,#15092,#15093,#15094,
#15095));
#6300=EDGE_LOOP('',(#15096,#15097,#15098,#15099));
#6301=EDGE_LOOP('',(#15100,#15101,#15102,#15103));
#6302=EDGE_LOOP('',(#15104,#15105,#15106,#15107));
#6303=EDGE_LOOP('',(#15108,#15109,#15110,#15111));
#6304=EDGE_LOOP('',(#15112,#15113,#15114,#15115));
#6305=EDGE_LOOP('',(#15116,#15117,#15118,#15119));
#6306=EDGE_LOOP('',(#15120,#15121,#15122,#15123));
#6307=EDGE_LOOP('',(#15124,#15125,#15126,#15127));
#6308=EDGE_LOOP('',(#15128,#15129,#15130,#15131));
#6309=EDGE_LOOP('',(#15132,#15133,#15134,#15135));
#6310=EDGE_LOOP('',(#15136,#15137,#15138,#15139));
#6311=EDGE_LOOP('',(#15140,#15141,#15142,#15143));
#6312=EDGE_LOOP('',(#15144,#15145,#15146,#15147));
#6313=EDGE_LOOP('',(#15148,#15149,#15150,#15151));
#6314=EDGE_LOOP('',(#15152,#15153,#15154,#15155));
#6315=EDGE_LOOP('',(#15156,#15157,#15158,#15159));
#6316=EDGE_LOOP('',(#15160,#15161,#15162,#15163));
#6317=EDGE_LOOP('',(#15164,#15165,#15166,#15167));
#6318=EDGE_LOOP('',(#15168,#15169,#15170,#15171));
#6319=EDGE_LOOP('',(#15172,#15173,#15174,#15175));
#6320=EDGE_LOOP('',(#15176,#15177,#15178,#15179));
#6321=EDGE_LOOP('',(#15180,#15181,#15182,#15183));
#6322=EDGE_LOOP('',(#15184,#15185,#15186,#15187));
#6323=EDGE_LOOP('',(#15188,#15189,#15190,#15191));
#6324=EDGE_LOOP('',(#15192,#15193,#15194,#15195));
#6325=EDGE_LOOP('',(#15196,#15197,#15198,#15199));
#6326=EDGE_LOOP('',(#15200,#15201,#15202,#15203,#15204,#15205,#15206,#15207,
#15208,#15209,#15210,#15211,#15212,#15213,#15214,#15215,#15216,#15217,#15218,
#15219,#15220,#15221,#15222,#15223,#15224,#15225,#15226,#15227,#15228,#15229,
#15230,#15231,#15232,#15233));
#6327=EDGE_LOOP('',(#15234,#15235,#15236,#15237));
#6328=EDGE_LOOP('',(#15238,#15239,#15240,#15241));
#6329=EDGE_LOOP('',(#15242,#15243,#15244,#15245));
#6330=EDGE_LOOP('',(#15246,#15247,#15248,#15249));
#6331=EDGE_LOOP('',(#15250,#15251,#15252,#15253));
#6332=EDGE_LOOP('',(#15254,#15255,#15256,#15257));
#6333=EDGE_LOOP('',(#15258,#15259,#15260,#15261));
#6334=EDGE_LOOP('',(#15262,#15263,#15264,#15265));
#6335=EDGE_LOOP('',(#15266,#15267,#15268,#15269,#15270,#15271,#15272,#15273,
#15274,#15275,#15276,#15277,#15278,#15279,#15280,#15281,#15282,#15283,#15284,
#15285,#15286,#15287,#15288,#15289,#15290,#15291,#15292,#15293,#15294,#15295,
#15296,#15297,#15298,#15299));
#6336=EDGE_LOOP('',(#15300,#15301,#15302,#15303));
#6337=EDGE_LOOP('',(#15304,#15305,#15306,#15307,#15308,#15309));
#6338=EDGE_LOOP('',(#15310,#15311,#15312,#15313));
#6339=EDGE_LOOP('',(#15314,#15315,#15316,#15317,#15318,#15319));
#6340=EDGE_LOOP('',(#15320,#15321,#15322,#15323));
#6341=EDGE_LOOP('',(#15324,#15325,#15326,#15327,#15328,#15329));
#6342=EDGE_LOOP('',(#15330,#15331,#15332,#15333));
#6343=EDGE_LOOP('',(#15334,#15335,#15336,#15337,#15338,#15339));
#6344=EDGE_LOOP('',(#15340,#15341,#15342,#15343));
#6345=EDGE_LOOP('',(#15344,#15345,#15346,#15347));
#6346=EDGE_LOOP('',(#15348,#15349,#15350,#15351));
#6347=EDGE_LOOP('',(#15352,#15353,#15354,#15355));
#6348=EDGE_LOOP('',(#15356,#15357,#15358,#15359));
#6349=EDGE_LOOP('',(#15360,#15361,#15362,#15363,#15364,#15365));
#6350=EDGE_LOOP('',(#15366,#15367,#15368,#15369));
#6351=EDGE_LOOP('',(#15370,#15371,#15372,#15373,#15374,#15375));
#6352=EDGE_LOOP('',(#15376,#15377,#15378,#15379));
#6353=EDGE_LOOP('',(#15380,#15381,#15382,#15383,#15384,#15385,#15386,#15387,
#15388,#15389,#15390,#15391,#15392,#15393,#15394,#15395));
#6354=EDGE_LOOP('',(#15396,#15397,#15398,#15399,#15400,#15401,#15402,#15403));
#6355=EDGE_LOOP('',(#15404));
#6356=EDGE_LOOP('',(#15405));
#6357=EDGE_LOOP('',(#15406));
#6358=EDGE_LOOP('',(#15407));
#6359=EDGE_LOOP('',(#15408,#15409,#15410,#15411,#15412,#15413));
#6360=EDGE_LOOP('',(#15414,#15415,#15416,#15417,#15418,#15419,#15420,#15421));
#6361=EDGE_LOOP('',(#15422));
#6362=EDGE_LOOP('',(#15423));
#6363=EDGE_LOOP('',(#15424));
#6364=EDGE_LOOP('',(#15425));
#6365=EDGE_LOOP('',(#15426));
#6366=EDGE_LOOP('',(#15427,#15428,#15429,#15430));
#6367=EDGE_LOOP('',(#15431,#15432,#15433,#15434));
#6368=EDGE_LOOP('',(#15435,#15436,#15437,#15438));
#6369=EDGE_LOOP('',(#15439,#15440,#15441,#15442));
#6370=EDGE_LOOP('',(#15443,#15444,#15445,#15446));
#6371=EDGE_LOOP('',(#15447,#15448,#15449,#15450));
#6372=EDGE_LOOP('',(#15451,#15452,#15453,#15454));
#6373=EDGE_LOOP('',(#15455,#15456,#15457,#15458));
#6374=EDGE_LOOP('',(#15459,#15460,#15461,#15462));
#6375=EDGE_LOOP('',(#15463,#15464,#15465,#15466));
#6376=EDGE_LOOP('',(#15467,#15468,#15469,#15470));
#6377=EDGE_LOOP('',(#15471,#15472,#15473,#15474));
#6378=EDGE_LOOP('',(#15475,#15476,#15477,#15478,#15479,#15480,#15481,#15482));
#6379=EDGE_LOOP('',(#15483));
#6380=EDGE_LOOP('',(#15484,#15485,#15486,#15487,#15488,#15489));
#6381=EDGE_LOOP('',(#15490,#15491,#15492,#15493,#15494));
#6382=EDGE_LOOP('',(#15495));
#6383=EDGE_LOOP('',(#15496));
#6384=EDGE_LOOP('',(#15497,#15498,#15499,#15500,#15501));
#6385=EDGE_LOOP('',(#15502,#15503,#15504,#15505,#15506));
#6386=EDGE_LOOP('',(#15507,#15508,#15509,#15510,#15511));
#6387=EDGE_LOOP('',(#15512,#15513,#15514,#15515));
#6388=EDGE_LOOP('',(#15516));
#6389=EDGE_LOOP('',(#15517));
#6390=EDGE_LOOP('',(#15518,#15519,#15520,#15521));
#6391=EDGE_LOOP('',(#15522));
#6392=EDGE_LOOP('',(#15523));
#6393=EDGE_LOOP('',(#15524,#15525,#15526,#15527));
#6394=EDGE_LOOP('',(#15528,#15529,#15530,#15531,#15532));
#6395=EDGE_LOOP('',(#15533,#15534,#15535,#15536,#15537));
#6396=EDGE_LOOP('',(#15538,#15539,#15540,#15541));
#6397=EDGE_LOOP('',(#15542,#15543,#15544,#15545));
#6398=EDGE_LOOP('',(#15546,#15547,#15548,#15549));
#6399=EDGE_LOOP('',(#15550,#15551,#15552,#15553));
#6400=EDGE_LOOP('',(#15554,#15555,#15556,#15557));
#6401=EDGE_LOOP('',(#15558));
#6402=EDGE_LOOP('',(#15559));
#6403=EDGE_LOOP('',(#15560,#15561,#15562,#15563));
#6404=EDGE_LOOP('',(#15564,#15565,#15566,#15567));
#6405=EDGE_LOOP('',(#15568,#15569,#15570,#15571));
#6406=EDGE_LOOP('',(#15572,#15573,#15574,#15575));
#6407=EDGE_LOOP('',(#15576,#15577,#15578,#15579));
#6408=EDGE_LOOP('',(#15580,#15581,#15582,#15583));
#6409=EDGE_LOOP('',(#15584,#15585,#15586,#15587));
#6410=EDGE_LOOP('',(#15588,#15589,#15590,#15591));
#6411=EDGE_LOOP('',(#15592,#15593,#15594,#15595));
#6412=EDGE_LOOP('',(#15596,#15597,#15598,#15599));
#6413=EDGE_LOOP('',(#15600,#15601,#15602,#15603));
#6414=EDGE_LOOP('',(#15604,#15605,#15606,#15607));
#6415=EDGE_LOOP('',(#15608,#15609,#15610,#15611));
#6416=EDGE_LOOP('',(#15612,#15613,#15614,#15615));
#6417=EDGE_LOOP('',(#15616,#15617,#15618,#15619));
#6418=EDGE_LOOP('',(#15620,#15621,#15622,#15623));
#6419=EDGE_LOOP('',(#15624,#15625,#15626,#15627));
#6420=EDGE_LOOP('',(#15628,#15629,#15630,#15631));
#6421=EDGE_LOOP('',(#15632,#15633,#15634,#15635));
#6422=EDGE_LOOP('',(#15636,#15637,#15638,#15639));
#6423=EDGE_LOOP('',(#15640,#15641,#15642,#15643));
#6424=EDGE_LOOP('',(#15644,#15645,#15646,#15647));
#6425=EDGE_LOOP('',(#15648,#15649,#15650,#15651));
#6426=EDGE_LOOP('',(#15652,#15653,#15654,#15655));
#6427=EDGE_LOOP('',(#15656,#15657,#15658,#15659));
#6428=EDGE_LOOP('',(#15660,#15661,#15662,#15663));
#6429=EDGE_LOOP('',(#15664,#15665,#15666,#15667));
#6430=EDGE_LOOP('',(#15668,#15669,#15670,#15671));
#6431=EDGE_LOOP('',(#15672,#15673,#15674,#15675));
#6432=EDGE_LOOP('',(#15676,#15677,#15678,#15679));
#6433=EDGE_LOOP('',(#15680,#15681,#15682,#15683));
#6434=EDGE_LOOP('',(#15684,#15685,#15686,#15687,#15688,#15689,#15690,#15691,
#15692,#15693,#15694,#15695,#15696,#15697,#15698,#15699,#15700,#15701,#15702,
#15703,#15704,#15705,#15706,#15707,#15708,#15709,#15710,#15711,#15712,#15713,
#15714,#15715,#15716,#15717));
#6435=EDGE_LOOP('',(#15718,#15719,#15720,#15721));
#6436=EDGE_LOOP('',(#15722,#15723,#15724,#15725));
#6437=EDGE_LOOP('',(#15726,#15727,#15728,#15729));
#6438=EDGE_LOOP('',(#15730,#15731,#15732,#15733));
#6439=EDGE_LOOP('',(#15734,#15735,#15736,#15737));
#6440=EDGE_LOOP('',(#15738,#15739,#15740,#15741));
#6441=EDGE_LOOP('',(#15742,#15743,#15744,#15745));
#6442=EDGE_LOOP('',(#15746,#15747,#15748,#15749));
#6443=EDGE_LOOP('',(#15750,#15751,#15752,#15753,#15754,#15755,#15756,#15757,
#15758,#15759,#15760,#15761,#15762,#15763,#15764,#15765,#15766,#15767,#15768,
#15769,#15770,#15771,#15772,#15773,#15774,#15775,#15776,#15777,#15778,#15779,
#15780,#15781,#15782,#15783));
#6444=EDGE_LOOP('',(#15784,#15785,#15786,#15787,#15788));
#6445=EDGE_LOOP('',(#15789,#15790,#15791,#15792));
#6446=EDGE_LOOP('',(#15793,#15794,#15795,#15796));
#6447=EDGE_LOOP('',(#15797));
#6448=EDGE_LOOP('',(#15798));
#6449=EDGE_LOOP('',(#15799));
#6450=EDGE_LOOP('',(#15800));
#6451=EDGE_LOOP('',(#15801,#15802,#15803,#15804,#15805,#15806,#15807,#15808,
#15809));
#6452=EDGE_LOOP('',(#15810,#15811,#15812,#15813,#15814));
#6453=EDGE_LOOP('',(#15815,#15816));
#6454=EDGE_LOOP('',(#15817,#15818,#15819,#15820,#15821));
#6455=EDGE_LOOP('',(#15822,#15823,#15824,#15825,#15826));
#6456=EDGE_LOOP('',(#15827));
#6457=EDGE_LOOP('',(#15828,#15829));
#6458=EDGE_LOOP('',(#15830,#15831,#15832,#15833));
#6459=EDGE_LOOP('',(#15834,#15835,#15836,#15837));
#6460=EDGE_LOOP('',(#15838,#15839,#15840,#15841));
#6461=EDGE_LOOP('',(#15842,#15843,#15844,#15845));
#6462=EDGE_LOOP('',(#15846,#15847,#15848,#15849));
#6463=EDGE_LOOP('',(#15850,#15851,#15852,#15853,#15854,#15855,#15856,#15857,
#15858,#15859,#15860,#15861,#15862,#15863));
#6464=EDGE_LOOP('',(#15864,#15865,#15866,#15867));
#6465=EDGE_LOOP('',(#15868,#15869,#15870,#15871));
#6466=EDGE_LOOP('',(#15872,#15873,#15874,#15875));
#6467=EDGE_LOOP('',(#15876,#15877,#15878,#15879));
#6468=EDGE_LOOP('',(#15880,#15881,#15882,#15883));
#6469=EDGE_LOOP('',(#15884,#15885,#15886,#15887));
#6470=EDGE_LOOP('',(#15888,#15889,#15890,#15891));
#6471=EDGE_LOOP('',(#15892,#15893,#15894,#15895));
#6472=EDGE_LOOP('',(#15896,#15897,#15898,#15899));
#6473=EDGE_LOOP('',(#15900,#15901,#15902,#15903,#15904,#15905,#15906,#15907,
#15908,#15909,#15910,#15911,#15912,#15913));
#6474=EDGE_LOOP('',(#15914,#15915,#15916,#15917));
#6475=EDGE_LOOP('',(#15918,#15919,#15920,#15921));
#6476=EDGE_LOOP('',(#15922,#15923,#15924,#15925));
#6477=EDGE_LOOP('',(#15926,#15927,#15928,#15929));
#6478=EDGE_LOOP('',(#15930,#15931,#15932,#15933));
#6479=EDGE_LOOP('',(#15934,#15935,#15936,#15937));
#6480=EDGE_LOOP('',(#15938,#15939,#15940,#15941));
#6481=EDGE_LOOP('',(#15942,#15943,#15944,#15945));
#6482=EDGE_LOOP('',(#15946,#15947,#15948,#15949));
#6483=EDGE_LOOP('',(#15950,#15951,#15952,#15953));
#6484=EDGE_LOOP('',(#15954,#15955,#15956,#15957));
#6485=EDGE_LOOP('',(#15958,#15959,#15960,#15961));
#6486=EDGE_LOOP('',(#15962,#15963,#15964,#15965));
#6487=EDGE_LOOP('',(#15966,#15967,#15968,#15969));
#6488=EDGE_LOOP('',(#15970,#15971,#15972,#15973));
#6489=EDGE_LOOP('',(#15974,#15975,#15976,#15977));
#6490=EDGE_LOOP('',(#15978,#15979,#15980,#15981));
#6491=EDGE_LOOP('',(#15982,#15983,#15984,#15985));
#6492=EDGE_LOOP('',(#15986,#15987,#15988,#15989));
#6493=EDGE_LOOP('',(#15990,#15991,#15992,#15993));
#6494=EDGE_LOOP('',(#15994,#15995,#15996,#15997,#15998,#15999,#16000,#16001,
#16002,#16003));
#6495=EDGE_LOOP('',(#16004));
#6496=EDGE_LOOP('',(#16005));
#6497=EDGE_LOOP('',(#16006));
#6498=EDGE_LOOP('',(#16007));
#6499=EDGE_LOOP('',(#16008));
#6500=EDGE_LOOP('',(#16009));
#6501=EDGE_LOOP('',(#16010));
#6502=EDGE_LOOP('',(#16011));
#6503=EDGE_LOOP('',(#16012));
#6504=EDGE_LOOP('',(#16013));
#6505=EDGE_LOOP('',(#16014,#16015,#16016,#16017,#16018,#16019,#16020,#16021,
#16022,#16023));
#6506=EDGE_LOOP('',(#16024));
#6507=EDGE_LOOP('',(#16025));
#6508=EDGE_LOOP('',(#16026));
#6509=EDGE_LOOP('',(#16027));
#6510=EDGE_LOOP('',(#16028));
#6511=EDGE_LOOP('',(#16029));
#6512=EDGE_LOOP('',(#16030));
#6513=EDGE_LOOP('',(#16031));
#6514=EDGE_LOOP('',(#16032));
#6515=EDGE_LOOP('',(#16033));
#6516=EDGE_LOOP('',(#16034,#16035,#16036,#16037));
#6517=EDGE_LOOP('',(#16038,#16039,#16040,#16041));
#6518=EDGE_LOOP('',(#16042,#16043,#16044,#16045));
#6519=EDGE_LOOP('',(#16046,#16047,#16048,#16049));
#6520=EDGE_LOOP('',(#16050,#16051,#16052,#16053));
#6521=EDGE_LOOP('',(#16054,#16055,#16056,#16057,#16058,#16059,#16060));
#6522=EDGE_LOOP('',(#16061,#16062,#16063,#16064));
#6523=EDGE_LOOP('',(#16065,#16066,#16067,#16068,#16069,#16070,#16071));
#6524=EDGE_LOOP('',(#16072,#16073,#16074,#16075));
#6525=EDGE_LOOP('',(#16076,#16077,#16078,#16079));
#6526=EDGE_LOOP('',(#16080,#16081,#16082,#16083));
#6527=EDGE_LOOP('',(#16084,#16085,#16086,#16087));
#6528=EDGE_LOOP('',(#16088,#16089,#16090,#16091));
#6529=EDGE_LOOP('',(#16092,#16093,#16094,#16095));
#6530=EDGE_LOOP('',(#16096,#16097,#16098,#16099));
#6531=EDGE_LOOP('',(#16100,#16101,#16102,#16103));
#6532=EDGE_LOOP('',(#16104,#16105,#16106,#16107));
#6533=EDGE_LOOP('',(#16108,#16109,#16110,#16111));
#6534=EDGE_LOOP('',(#16112,#16113,#16114,#16115));
#6535=EDGE_LOOP('',(#16116,#16117,#16118,#16119));
#6536=EDGE_LOOP('',(#16120,#16121,#16122,#16123));
#6537=EDGE_LOOP('',(#16124,#16125,#16126,#16127));
#6538=EDGE_LOOP('',(#16128,#16129,#16130,#16131));
#6539=EDGE_LOOP('',(#16132,#16133,#16134,#16135));
#6540=EDGE_LOOP('',(#16136,#16137,#16138,#16139));
#6541=EDGE_LOOP('',(#16140,#16141,#16142,#16143));
#6542=EDGE_LOOP('',(#16144,#16145,#16146,#16147));
#6543=EDGE_LOOP('',(#16148,#16149,#16150,#16151));
#6544=EDGE_LOOP('',(#16152,#16153,#16154,#16155));
#6545=EDGE_LOOP('',(#16156,#16157,#16158,#16159));
#6546=EDGE_LOOP('',(#16160,#16161,#16162,#16163));
#6547=EDGE_LOOP('',(#16164,#16165,#16166,#16167));
#6548=EDGE_LOOP('',(#16168,#16169,#16170,#16171));
#6549=EDGE_LOOP('',(#16172,#16173,#16174,#16175));
#6550=EDGE_LOOP('',(#16176,#16177,#16178,#16179));
#6551=EDGE_LOOP('',(#16180,#16181,#16182,#16183,#16184,#16185,#16186,#16187,
#16188,#16189,#16190,#16191,#16192,#16193,#16194,#16195,#16196,#16197,#16198,
#16199,#16200,#16201,#16202,#16203,#16204,#16205,#16206,#16207,#16208,#16209,
#16210,#16211,#16212,#16213));
#6552=EDGE_LOOP('',(#16214,#16215,#16216,#16217));
#6553=EDGE_LOOP('',(#16218,#16219,#16220,#16221));
#6554=EDGE_LOOP('',(#16222,#16223,#16224,#16225));
#6555=EDGE_LOOP('',(#16226,#16227,#16228,#16229));
#6556=EDGE_LOOP('',(#16230,#16231,#16232,#16233));
#6557=EDGE_LOOP('',(#16234,#16235,#16236,#16237));
#6558=EDGE_LOOP('',(#16238,#16239,#16240,#16241));
#6559=EDGE_LOOP('',(#16242,#16243,#16244,#16245));
#6560=EDGE_LOOP('',(#16246,#16247,#16248,#16249,#16250,#16251,#16252,#16253,
#16254,#16255,#16256,#16257,#16258,#16259,#16260,#16261,#16262,#16263,#16264,
#16265,#16266,#16267,#16268,#16269,#16270,#16271,#16272,#16273,#16274,#16275,
#16276,#16277,#16278,#16279));
#6561=EDGE_LOOP('',(#16280));
#6562=EDGE_LOOP('',(#16281));
#6563=EDGE_LOOP('',(#16282,#16283,#16284,#16285));
#6564=EDGE_LOOP('',(#16286,#16287,#16288,#16289));
#6565=EDGE_LOOP('',(#16290));
#6566=EDGE_LOOP('',(#16291));
#6567=EDGE_LOOP('',(#16292,#16293,#16294,#16295));
#6568=EDGE_LOOP('',(#16296,#16297,#16298,#16299));
#6569=EDGE_LOOP('',(#16300,#16301,#16302,#16303,#16304,#16305,#16306));
#6570=EDGE_LOOP('',(#16307,#16308,#16309,#16310));
#6571=EDGE_LOOP('',(#16311,#16312,#16313,#16314,#16315,#16316,#16317));
#6572=EDGE_LOOP('',(#16318,#16319,#16320,#16321));
#6573=EDGE_LOOP('',(#16322,#16323,#16324,#16325));
#6574=EDGE_LOOP('',(#16326,#16327,#16328,#16329));
#6575=EDGE_LOOP('',(#16330,#16331,#16332,#16333));
#6576=EDGE_LOOP('',(#16334,#16335,#16336,#16337));
#6577=EDGE_LOOP('',(#16338,#16339,#16340,#16341));
#6578=EDGE_LOOP('',(#16342,#16343,#16344,#16345));
#6579=EDGE_LOOP('',(#16346,#16347,#16348,#16349));
#6580=EDGE_LOOP('',(#16350,#16351,#16352,#16353));
#6581=EDGE_LOOP('',(#16354,#16355,#16356,#16357));
#6582=EDGE_LOOP('',(#16358,#16359,#16360,#16361));
#6583=EDGE_LOOP('',(#16362,#16363,#16364,#16365));
#6584=EDGE_LOOP('',(#16366,#16367,#16368,#16369));
#6585=EDGE_LOOP('',(#16370,#16371,#16372,#16373));
#6586=EDGE_LOOP('',(#16374,#16375,#16376,#16377));
#6587=EDGE_LOOP('',(#16378,#16379,#16380,#16381));
#6588=EDGE_LOOP('',(#16382,#16383,#16384,#16385));
#6589=EDGE_LOOP('',(#16386,#16387,#16388,#16389));
#6590=EDGE_LOOP('',(#16390,#16391,#16392,#16393));
#6591=EDGE_LOOP('',(#16394,#16395,#16396,#16397));
#6592=EDGE_LOOP('',(#16398,#16399,#16400,#16401));
#6593=EDGE_LOOP('',(#16402,#16403,#16404,#16405));
#6594=EDGE_LOOP('',(#16406,#16407,#16408,#16409));
#6595=EDGE_LOOP('',(#16410,#16411,#16412,#16413));
#6596=EDGE_LOOP('',(#16414,#16415,#16416,#16417));
#6597=EDGE_LOOP('',(#16418,#16419,#16420,#16421));
#6598=EDGE_LOOP('',(#16422,#16423,#16424,#16425));
#6599=EDGE_LOOP('',(#16426,#16427,#16428,#16429));
#6600=EDGE_LOOP('',(#16430,#16431,#16432,#16433));
#6601=EDGE_LOOP('',(#16434,#16435,#16436,#16437));
#6602=EDGE_LOOP('',(#16438,#16439,#16440,#16441));
#6603=EDGE_LOOP('',(#16442,#16443,#16444,#16445));
#6604=EDGE_LOOP('',(#16446,#16447,#16448,#16449));
#6605=EDGE_LOOP('',(#16450,#16451,#16452,#16453));
#6606=EDGE_LOOP('',(#16454,#16455,#16456,#16457));
#6607=EDGE_LOOP('',(#16458,#16459,#16460,#16461));
#6608=EDGE_LOOP('',(#16462,#16463,#16464,#16465));
#6609=EDGE_LOOP('',(#16466,#16467,#16468,#16469));
#6610=EDGE_LOOP('',(#16470,#16471,#16472,#16473));
#6611=EDGE_LOOP('',(#16474,#16475,#16476,#16477));
#6612=EDGE_LOOP('',(#16478,#16479,#16480,#16481));
#6613=EDGE_LOOP('',(#16482,#16483,#16484,#16485));
#6614=EDGE_LOOP('',(#16486,#16487,#16488,#16489));
#6615=EDGE_LOOP('',(#16490,#16491,#16492,#16493));
#6616=EDGE_LOOP('',(#16494,#16495,#16496,#16497));
#6617=EDGE_LOOP('',(#16498,#16499,#16500,#16501));
#6618=EDGE_LOOP('',(#16502,#16503,#16504,#16505));
#6619=EDGE_LOOP('',(#16506,#16507,#16508,#16509));
#6620=EDGE_LOOP('',(#16510,#16511,#16512,#16513,#16514,#16515,#16516,#16517,
#16518,#16519,#16520,#16521,#16522,#16523,#16524,#16525,#16526,#16527,#16528,
#16529,#16530,#16531,#16532,#16533,#16534,#16535,#16536,#16537,#16538,#16539,
#16540,#16541,#16542,#16543,#16544,#16545,#16546,#16547,#16548,#16549,#16550,
#16551,#16552,#16553,#16554,#16555,#16556,#16557,#16558,#16559,#16560,#16561,
#16562,#16563,#16564,#16565,#16566,#16567,#16568,#16569,#16570,#16571,#16572,
#16573,#16574,#16575,#16576,#16577,#16578,#16579,#16580,#16581,#16582,#16583,
#16584,#16585,#16586,#16587,#16588,#16589,#16590,#16591,#16592,#16593,#16594,
#16595,#16596,#16597,#16598,#16599));
#6621=EDGE_LOOP('',(#16600));
#6622=EDGE_LOOP('',(#16601,#16602,#16603,#16604));
#6623=EDGE_LOOP('',(#16605,#16606,#16607,#16608));
#6624=EDGE_LOOP('',(#16609,#16610,#16611,#16612));
#6625=EDGE_LOOP('',(#16613,#16614,#16615,#16616));
#6626=EDGE_LOOP('',(#16617,#16618,#16619,#16620));
#6627=EDGE_LOOP('',(#16621,#16622,#16623,#16624));
#6628=EDGE_LOOP('',(#16625,#16626,#16627,#16628));
#6629=EDGE_LOOP('',(#16629,#16630,#16631,#16632));
#6630=EDGE_LOOP('',(#16633,#16634,#16635,#16636));
#6631=EDGE_LOOP('',(#16637,#16638,#16639,#16640));
#6632=EDGE_LOOP('',(#16641,#16642,#16643,#16644));
#6633=EDGE_LOOP('',(#16645,#16646,#16647,#16648));
#6634=EDGE_LOOP('',(#16649,#16650,#16651,#16652));
#6635=EDGE_LOOP('',(#16653,#16654,#16655,#16656));
#6636=EDGE_LOOP('',(#16657,#16658,#16659,#16660));
#6637=EDGE_LOOP('',(#16661,#16662,#16663,#16664));
#6638=EDGE_LOOP('',(#16665,#16666,#16667,#16668));
#6639=EDGE_LOOP('',(#16669,#16670,#16671,#16672));
#6640=EDGE_LOOP('',(#16673,#16674,#16675,#16676));
#6641=EDGE_LOOP('',(#16677,#16678,#16679,#16680));
#6642=EDGE_LOOP('',(#16681,#16682,#16683,#16684));
#6643=EDGE_LOOP('',(#16685,#16686,#16687,#16688));
#6644=EDGE_LOOP('',(#16689,#16690,#16691,#16692));
#6645=EDGE_LOOP('',(#16693,#16694,#16695,#16696));
#6646=EDGE_LOOP('',(#16697,#16698,#16699,#16700));
#6647=EDGE_LOOP('',(#16701,#16702,#16703,#16704));
#6648=EDGE_LOOP('',(#16705,#16706,#16707,#16708));
#6649=EDGE_LOOP('',(#16709,#16710,#16711,#16712));
#6650=EDGE_LOOP('',(#16713,#16714,#16715,#16716));
#6651=EDGE_LOOP('',(#16717,#16718,#16719,#16720));
#6652=EDGE_LOOP('',(#16721,#16722,#16723,#16724));
#6653=EDGE_LOOP('',(#16725,#16726,#16727,#16728));
#6654=EDGE_LOOP('',(#16729,#16730,#16731,#16732));
#6655=EDGE_LOOP('',(#16733,#16734,#16735,#16736));
#6656=EDGE_LOOP('',(#16737,#16738,#16739,#16740));
#6657=EDGE_LOOP('',(#16741,#16742,#16743,#16744));
#6658=EDGE_LOOP('',(#16745,#16746,#16747,#16748));
#6659=EDGE_LOOP('',(#16749,#16750,#16751,#16752));
#6660=EDGE_LOOP('',(#16753,#16754,#16755,#16756));
#6661=EDGE_LOOP('',(#16757,#16758,#16759,#16760));
#6662=EDGE_LOOP('',(#16761,#16762,#16763,#16764));
#6663=EDGE_LOOP('',(#16765,#16766,#16767,#16768));
#6664=EDGE_LOOP('',(#16769,#16770,#16771,#16772));
#6665=EDGE_LOOP('',(#16773,#16774,#16775,#16776));
#6666=EDGE_LOOP('',(#16777,#16778,#16779,#16780));
#6667=EDGE_LOOP('',(#16781,#16782,#16783,#16784,#16785,#16786,#16787,#16788,
#16789,#16790,#16791,#16792,#16793,#16794,#16795,#16796,#16797,#16798,#16799,
#16800,#16801,#16802,#16803,#16804,#16805,#16806,#16807,#16808,#16809,#16810,
#16811,#16812,#16813,#16814,#16815,#16816,#16817,#16818,#16819,#16820,#16821,
#16822,#16823,#16824,#16825,#16826,#16827,#16828,#16829,#16830,#16831,#16832,
#16833,#16834,#16835,#16836,#16837,#16838,#16839,#16840,#16841,#16842,#16843,
#16844,#16845,#16846,#16847,#16848,#16849,#16850,#16851,#16852,#16853,#16854,
#16855,#16856,#16857,#16858,#16859,#16860,#16861,#16862,#16863,#16864,#16865,
#16866,#16867,#16868,#16869,#16870));
#6668=EDGE_LOOP('',(#16871));
#6669=EDGE_LOOP('',(#16872,#16873,#16874,#16875));
#6670=EDGE_LOOP('',(#16876,#16877,#16878,#16879));
#6671=EDGE_LOOP('',(#16880,#16881,#16882,#16883,#16884));
#6672=EDGE_LOOP('',(#16885,#16886,#16887,#16888,#16889,#16890));
#6673=EDGE_LOOP('',(#16891));
#6674=EDGE_LOOP('',(#16892));
#6675=EDGE_LOOP('',(#16893,#16894,#16895,#16896,#16897));
#6676=EDGE_LOOP('',(#16898));
#6677=EDGE_LOOP('',(#16899));
#6678=EDGE_LOOP('',(#16900,#16901,#16902,#16903));
#6679=EDGE_LOOP('',(#16904,#16905,#16906,#16907));
#6680=EDGE_LOOP('',(#16908,#16909,#16910,#16911));
#6681=EDGE_LOOP('',(#16912,#16913,#16914,#16915));
#6682=EDGE_LOOP('',(#16916,#16917,#16918,#16919));
#6683=EDGE_LOOP('',(#16920,#16921,#16922,#16923));
#6684=EDGE_LOOP('',(#16924,#16925,#16926,#16927));
#6685=EDGE_LOOP('',(#16928,#16929,#16930,#16931));
#6686=EDGE_LOOP('',(#16932,#16933,#16934,#16935));
#6687=EDGE_LOOP('',(#16936,#16937,#16938,#16939));
#6688=EDGE_LOOP('',(#16940,#16941,#16942,#16943));
#6689=EDGE_LOOP('',(#16944,#16945,#16946,#16947));
#6690=EDGE_LOOP('',(#16948,#16949,#16950,#16951));
#6691=EDGE_LOOP('',(#16952,#16953,#16954,#16955));
#6692=EDGE_LOOP('',(#16956,#16957,#16958,#16959));
#6693=EDGE_LOOP('',(#16960,#16961,#16962,#16963));
#6694=EDGE_LOOP('',(#16964,#16965,#16966,#16967));
#6695=EDGE_LOOP('',(#16968,#16969,#16970,#16971));
#6696=EDGE_LOOP('',(#16972,#16973,#16974,#16975));
#6697=EDGE_LOOP('',(#16976,#16977,#16978,#16979));
#6698=EDGE_LOOP('',(#16980,#16981,#16982,#16983));
#6699=EDGE_LOOP('',(#16984,#16985,#16986,#16987));
#6700=EDGE_LOOP('',(#16988,#16989,#16990,#16991));
#6701=EDGE_LOOP('',(#16992,#16993,#16994,#16995));
#6702=EDGE_LOOP('',(#16996,#16997,#16998,#16999));
#6703=EDGE_LOOP('',(#17000,#17001,#17002,#17003));
#6704=EDGE_LOOP('',(#17004,#17005,#17006,#17007));
#6705=EDGE_LOOP('',(#17008,#17009,#17010,#17011,#17012,#17013,#17014,#17015,
#17016,#17017,#17018,#17019,#17020,#17021,#17022,#17023,#17024,#17025,#17026,
#17027,#17028,#17029,#17030,#17031,#17032,#17033,#17034,#17035,#17036,#17037,
#17038,#17039,#17040,#17041));
#6706=EDGE_LOOP('',(#17042,#17043,#17044,#17045));
#6707=EDGE_LOOP('',(#17046,#17047,#17048,#17049));
#6708=EDGE_LOOP('',(#17050,#17051,#17052,#17053));
#6709=EDGE_LOOP('',(#17054,#17055,#17056,#17057));
#6710=EDGE_LOOP('',(#17058,#17059,#17060,#17061));
#6711=EDGE_LOOP('',(#17062,#17063,#17064,#17065));
#6712=EDGE_LOOP('',(#17066,#17067,#17068,#17069));
#6713=EDGE_LOOP('',(#17070,#17071,#17072,#17073));
#6714=EDGE_LOOP('',(#17074,#17075,#17076,#17077,#17078,#17079,#17080,#17081,
#17082,#17083,#17084,#17085,#17086,#17087,#17088,#17089,#17090,#17091,#17092,
#17093,#17094,#17095,#17096,#17097,#17098,#17099,#17100,#17101,#17102,#17103,
#17104,#17105,#17106,#17107));
#6715=EDGE_LOOP('',(#17108,#17109,#17110,#17111));
#6716=EDGE_LOOP('',(#17112,#17113,#17114,#17115));
#6717=EDGE_LOOP('',(#17116,#17117,#17118,#17119));
#6718=EDGE_LOOP('',(#17120,#17121,#17122,#17123,#17124,#17125,#17126));
#6719=EDGE_LOOP('',(#17127,#17128,#17129,#17130));
#6720=EDGE_LOOP('',(#17131,#17132,#17133,#17134,#17135,#17136,#17137));
#6721=EDGE_LOOP('',(#17138,#17139,#17140,#17141));
#6722=EDGE_LOOP('',(#17142,#17143,#17144,#17145));
#6723=EDGE_LOOP('',(#17146,#17147,#17148,#17149));
#6724=EDGE_LOOP('',(#17150,#17151,#17152,#17153));
#6725=EDGE_LOOP('',(#17154,#17155,#17156,#17157));
#6726=EDGE_LOOP('',(#17158,#17159,#17160,#17161));
#6727=EDGE_LOOP('',(#17162,#17163,#17164,#17165));
#6728=EDGE_LOOP('',(#17166,#17167,#17168,#17169));
#6729=EDGE_LOOP('',(#17170,#17171,#17172,#17173));
#6730=EDGE_LOOP('',(#17174,#17175,#17176,#17177));
#6731=EDGE_LOOP('',(#17178,#17179,#17180,#17181));
#6732=EDGE_LOOP('',(#17182,#17183,#17184,#17185));
#6733=EDGE_LOOP('',(#17186,#17187,#17188,#17189));
#6734=EDGE_LOOP('',(#17190,#17191,#17192,#17193));
#6735=EDGE_LOOP('',(#17194,#17195,#17196,#17197));
#6736=EDGE_LOOP('',(#17198,#17199,#17200,#17201));
#6737=EDGE_LOOP('',(#17202,#17203,#17204,#17205));
#6738=EDGE_LOOP('',(#17206,#17207,#17208,#17209));
#6739=EDGE_LOOP('',(#17210,#17211,#17212,#17213,#17214,#17215,#17216,#17217,
#17218,#17219,#17220,#17221,#17222,#17223,#17224,#17225));
#6740=EDGE_LOOP('',(#17226));
#6741=EDGE_LOOP('',(#17227));
#6742=EDGE_LOOP('',(#17228));
#6743=EDGE_LOOP('',(#17229));
#6744=EDGE_LOOP('',(#17230,#17231,#17232,#17233,#17234,#17235,#17236,#17237));
#6745=EDGE_LOOP('',(#17238,#17239,#17240,#17241));
#6746=EDGE_LOOP('',(#17242,#17243,#17244,#17245));
#6747=EDGE_LOOP('',(#17246,#17247,#17248,#17249));
#6748=EDGE_LOOP('',(#17250,#17251,#17252,#17253));
#6749=EDGE_LOOP('',(#17254,#17255,#17256,#17257));
#6750=EDGE_LOOP('',(#17258,#17259,#17260,#17261));
#6751=EDGE_LOOP('',(#17262,#17263,#17264,#17265));
#6752=EDGE_LOOP('',(#17266,#17267,#17268,#17269));
#6753=EDGE_LOOP('',(#17270,#17271,#17272,#17273));
#6754=EDGE_LOOP('',(#17274,#17275,#17276,#17277));
#6755=EDGE_LOOP('',(#17278,#17279,#17280,#17281));
#6756=EDGE_LOOP('',(#17282,#17283,#17284,#17285));
#6757=EDGE_LOOP('',(#17286,#17287,#17288,#17289));
#6758=EDGE_LOOP('',(#17290,#17291,#17292,#17293,#17294,#17295,#17296,#17297,
#17298,#17299,#17300,#17301,#17302,#17303,#17304,#17305));
#6759=EDGE_LOOP('',(#17306));
#6760=EDGE_LOOP('',(#17307));
#6761=EDGE_LOOP('',(#17308));
#6762=EDGE_LOOP('',(#17309));
#6763=EDGE_LOOP('',(#17310,#17311,#17312,#17313,#17314,#17315,#17316,#17317));
#6764=EDGE_LOOP('',(#17318,#17319,#17320,#17321));
#6765=EDGE_LOOP('',(#17322,#17323,#17324,#17325));
#6766=EDGE_LOOP('',(#17326,#17327,#17328,#17329));
#6767=EDGE_LOOP('',(#17330,#17331,#17332,#17333));
#6768=EDGE_LOOP('',(#17334,#17335,#17336,#17337));
#6769=EDGE_LOOP('',(#17338,#17339,#17340,#17341));
#6770=EDGE_LOOP('',(#17342,#17343,#17344,#17345));
#6771=EDGE_LOOP('',(#17346,#17347,#17348,#17349));
#6772=EDGE_LOOP('',(#17350,#17351,#17352,#17353));
#6773=EDGE_LOOP('',(#17354,#17355,#17356,#17357));
#6774=EDGE_LOOP('',(#17358,#17359,#17360,#17361));
#6775=EDGE_LOOP('',(#17362,#17363,#17364,#17365));
#6776=EDGE_LOOP('',(#17366,#17367,#17368,#17369));
#6777=EDGE_LOOP('',(#17370,#17371,#17372,#17373));
#6778=EDGE_LOOP('',(#17374,#17375,#17376,#17377));
#6779=EDGE_LOOP('',(#17378,#17379,#17380,#17381));
#6780=EDGE_LOOP('',(#17382,#17383,#17384,#17385));
#6781=EDGE_LOOP('',(#17386,#17387,#17388,#17389));
#6782=EDGE_LOOP('',(#17390,#17391,#17392,#17393));
#6783=EDGE_LOOP('',(#17394,#17395,#17396,#17397));
#6784=EDGE_LOOP('',(#17398,#17399,#17400,#17401));
#6785=EDGE_LOOP('',(#17402,#17403,#17404,#17405));
#6786=EDGE_LOOP('',(#17406,#17407,#17408,#17409));
#6787=EDGE_LOOP('',(#17410,#17411,#17412,#17413));
#6788=EDGE_LOOP('',(#17414,#17415,#17416,#17417));
#6789=EDGE_LOOP('',(#17418,#17419,#17420,#17421));
#6790=EDGE_LOOP('',(#17422,#17423,#17424,#17425,#17426,#17427,#17428,#17429,
#17430,#17431,#17432,#17433,#17434,#17435,#17436,#17437,#17438,#17439,#17440,
#17441,#17442,#17443,#17444,#17445,#17446,#17447,#17448,#17449,#17450,#17451,
#17452,#17453,#17454,#17455));
#6791=EDGE_LOOP('',(#17456,#17457,#17458,#17459));
#6792=EDGE_LOOP('',(#17460,#17461,#17462,#17463));
#6793=EDGE_LOOP('',(#17464,#17465,#17466,#17467));
#6794=EDGE_LOOP('',(#17468,#17469,#17470,#17471));
#6795=EDGE_LOOP('',(#17472,#17473,#17474,#17475));
#6796=EDGE_LOOP('',(#17476,#17477,#17478,#17479));
#6797=EDGE_LOOP('',(#17480,#17481,#17482,#17483));
#6798=EDGE_LOOP('',(#17484,#17485,#17486,#17487));
#6799=EDGE_LOOP('',(#17488,#17489,#17490,#17491,#17492,#17493,#17494,#17495,
#17496,#17497,#17498,#17499,#17500,#17501,#17502,#17503,#17504,#17505,#17506,
#17507,#17508,#17509,#17510,#17511,#17512,#17513,#17514,#17515,#17516,#17517,
#17518,#17519,#17520,#17521));
#6800=EDGE_LOOP('',(#17522,#17523,#17524,#17525));
#6801=EDGE_LOOP('',(#17526,#17527,#17528,#17529));
#6802=EDGE_LOOP('',(#17530,#17531,#17532,#17533));
#6803=EDGE_LOOP('',(#17534,#17535,#17536,#17537));
#6804=EDGE_LOOP('',(#17538,#17539,#17540,#17541));
#6805=EDGE_LOOP('',(#17542,#17543,#17544,#17545));
#6806=EDGE_LOOP('',(#17546,#17547,#17548,#17549));
#6807=EDGE_LOOP('',(#17550,#17551,#17552,#17553));
#6808=EDGE_LOOP('',(#17554,#17555,#17556,#17557));
#6809=EDGE_LOOP('',(#17558,#17559,#17560,#17561));
#6810=EDGE_LOOP('',(#17562,#17563,#17564,#17565));
#6811=EDGE_LOOP('',(#17566,#17567,#17568,#17569));
#6812=EDGE_LOOP('',(#17570,#17571,#17572,#17573));
#6813=EDGE_LOOP('',(#17574,#17575,#17576,#17577));
#6814=EDGE_LOOP('',(#17578,#17579,#17580,#17581));
#6815=EDGE_LOOP('',(#17582,#17583,#17584,#17585));
#6816=EDGE_LOOP('',(#17586,#17587,#17588,#17589));
#6817=EDGE_LOOP('',(#17590,#17591,#17592,#17593));
#6818=EDGE_LOOP('',(#17594,#17595,#17596,#17597));
#6819=EDGE_LOOP('',(#17598,#17599,#17600,#17601));
#6820=EDGE_LOOP('',(#17602,#17603,#17604,#17605));
#6821=EDGE_LOOP('',(#17606,#17607,#17608,#17609));
#6822=EDGE_LOOP('',(#17610,#17611,#17612,#17613));
#6823=EDGE_LOOP('',(#17614,#17615,#17616,#17617));
#6824=EDGE_LOOP('',(#17618,#17619,#17620,#17621));
#6825=EDGE_LOOP('',(#17622,#17623,#17624,#17625));
#6826=EDGE_LOOP('',(#17626,#17627,#17628,#17629));
#6827=EDGE_LOOP('',(#17630,#17631,#17632,#17633,#17634,#17635,#17636,#17637));
#6828=EDGE_LOOP('',(#17638,#17639,#17640,#17641,#17642,#17643));
#6829=EDGE_LOOP('',(#17644,#17645,#17646,#17647));
#6830=EDGE_LOOP('',(#17648,#17649,#17650,#17651,#17652,#17653,#17654,#17655,
#17656,#17657,#17658,#17659));
#6831=EDGE_LOOP('',(#17660,#17661,#17662,#17663));
#6832=EDGE_LOOP('',(#17664,#17665,#17666,#17667));
#6833=EDGE_LOOP('',(#17668,#17669,#17670,#17671));
#6834=EDGE_LOOP('',(#17672,#17673,#17674,#17675));
#6835=EDGE_LOOP('',(#17676,#17677,#17678,#17679));
#6836=EDGE_LOOP('',(#17680,#17681,#17682,#17683));
#6837=EDGE_LOOP('',(#17684,#17685,#17686,#17687));
#6838=EDGE_LOOP('',(#17688,#17689,#17690,#17691));
#6839=EDGE_LOOP('',(#17692,#17693,#17694,#17695,#17696));
#6840=EDGE_LOOP('',(#17697,#17698,#17699,#17700,#17701,#17702));
#6841=EDGE_LOOP('',(#17703,#17704,#17705,#17706,#17707,#17708,#17709,#17710,
#17711,#17712,#17713,#17714,#17715,#17716,#17717,#17718));
#6842=EDGE_LOOP('',(#17719,#17720,#17721,#17722));
#6843=EDGE_LOOP('',(#17723,#17724,#17725,#17726));
#6844=EDGE_LOOP('',(#17727,#17728,#17729,#17730,#17731));
#6845=EDGE_LOOP('',(#17732,#17733,#17734,#17735));
#6846=EDGE_LOOP('',(#17736,#17737,#17738,#17739));
#6847=EDGE_LOOP('',(#17740,#17741,#17742,#17743));
#6848=EDGE_LOOP('',(#17744,#17745,#17746,#17747,#17748,#17749,#17750,#17751));
#6849=EDGE_LOOP('',(#17752,#17753,#17754,#17755,#17756,#17757));
#6850=EDGE_LOOP('',(#17758,#17759,#17760,#17761,#17762,#17763,#17764,#17765));
#6851=EDGE_LOOP('',(#17766,#17767,#17768,#17769));
#6852=EDGE_LOOP('',(#17770,#17771,#17772,#17773,#17774,#17775,#17776,#17777,
#17778,#17779,#17780,#17781,#17782,#17783));
#6853=EDGE_LOOP('',(#17784,#17785,#17786,#17787));
#6854=EDGE_LOOP('',(#17788,#17789,#17790,#17791,#17792,#17793,#17794,#17795,
#17796,#17797,#17798,#17799,#17800,#17801));
#6855=EDGE_LOOP('',(#17802,#17803,#17804,#17805,#17806,#17807));
#6856=EDGE_LOOP('',(#17808,#17809,#17810,#17811));
#6857=EDGE_LOOP('',(#17812,#17813,#17814,#17815,#17816,#17817,#17818,#17819,
#17820,#17821));
#6858=EDGE_LOOP('',(#17822,#17823,#17824,#17825));
#6859=EDGE_LOOP('',(#17826,#17827,#17828,#17829));
#6860=EDGE_LOOP('',(#17830,#17831,#17832,#17833));
#6861=EDGE_LOOP('',(#17834,#17835,#17836,#17837));
#6862=EDGE_LOOP('',(#17838,#17839,#17840,#17841));
#6863=EDGE_LOOP('',(#17842,#17843,#17844,#17845));
#6864=EDGE_LOOP('',(#17846,#17847,#17848,#17849));
#6865=EDGE_LOOP('',(#17850,#17851,#17852,#17853));
#6866=EDGE_LOOP('',(#17854,#17855,#17856,#17857));
#6867=EDGE_LOOP('',(#17858,#17859,#17860,#17861));
#6868=EDGE_LOOP('',(#17862));
#6869=EDGE_LOOP('',(#17863));
#6870=EDGE_LOOP('',(#17864));
#6871=EDGE_LOOP('',(#17865));
#6872=EDGE_LOOP('',(#17866,#17867,#17868,#17869));
#6873=EDGE_LOOP('',(#17870,#17871,#17872,#17873));
#6874=EDGE_LOOP('',(#17874,#17875,#17876,#17877));
#6875=EDGE_LOOP('',(#17878,#17879,#17880,#17881));
#6876=EDGE_LOOP('',(#17882,#17883,#17884,#17885));
#6877=EDGE_LOOP('',(#17886,#17887,#17888,#17889));
#6878=EDGE_LOOP('',(#17890,#17891,#17892,#17893));
#6879=EDGE_LOOP('',(#17894,#17895,#17896,#17897));
#6880=EDGE_LOOP('',(#17898,#17899,#17900,#17901));
#6881=EDGE_LOOP('',(#17902,#17903,#17904,#17905));
#6882=EDGE_LOOP('',(#17906,#17907,#17908,#17909));
#6883=EDGE_LOOP('',(#17910,#17911,#17912,#17913));
#6884=EDGE_LOOP('',(#17914,#17915,#17916,#17917));
#6885=EDGE_LOOP('',(#17918,#17919,#17920,#17921));
#6886=EDGE_LOOP('',(#17922,#17923,#17924,#17925));
#6887=EDGE_LOOP('',(#17926,#17927,#17928,#17929));
#6888=EDGE_LOOP('',(#17930,#17931,#17932,#17933));
#6889=EDGE_LOOP('',(#17934,#17935,#17936,#17937));
#6890=EDGE_LOOP('',(#17938,#17939,#17940,#17941));
#6891=EDGE_LOOP('',(#17942,#17943,#17944,#17945));
#6892=EDGE_LOOP('',(#17946,#17947,#17948,#17949));
#6893=EDGE_LOOP('',(#17950,#17951,#17952,#17953));
#6894=EDGE_LOOP('',(#17954,#17955,#17956,#17957));
#6895=EDGE_LOOP('',(#17958,#17959,#17960,#17961));
#6896=EDGE_LOOP('',(#17962,#17963,#17964,#17965));
#6897=EDGE_LOOP('',(#17966,#17967,#17968,#17969));
#6898=EDGE_LOOP('',(#17970,#17971,#17972,#17973,#17974,#17975,#17976,#17977,
#17978,#17979,#17980,#17981,#17982,#17983,#17984,#17985,#17986,#17987,#17988,
#17989,#17990,#17991,#17992,#17993,#17994,#17995,#17996,#17997,#17998,#17999,
#18000,#18001,#18002,#18003));
#6899=EDGE_LOOP('',(#18004,#18005,#18006,#18007));
#6900=EDGE_LOOP('',(#18008,#18009,#18010,#18011));
#6901=EDGE_LOOP('',(#18012,#18013,#18014,#18015));
#6902=EDGE_LOOP('',(#18016,#18017,#18018,#18019));
#6903=EDGE_LOOP('',(#18020,#18021,#18022,#18023));
#6904=EDGE_LOOP('',(#18024,#18025,#18026,#18027));
#6905=EDGE_LOOP('',(#18028,#18029,#18030,#18031));
#6906=EDGE_LOOP('',(#18032,#18033,#18034,#18035));
#6907=EDGE_LOOP('',(#18036,#18037,#18038,#18039,#18040,#18041,#18042,#18043,
#18044,#18045,#18046,#18047,#18048,#18049,#18050,#18051,#18052,#18053,#18054,
#18055,#18056,#18057,#18058,#18059,#18060,#18061,#18062,#18063,#18064,#18065,
#18066,#18067,#18068,#18069));
#6908=EDGE_LOOP('',(#18070,#18071,#18072,#18073));
#6909=EDGE_LOOP('',(#18074,#18075,#18076,#18077));
#6910=EDGE_LOOP('',(#18078,#18079,#18080,#18081));
#6911=EDGE_LOOP('',(#18082,#18083,#18084,#18085));
#6912=EDGE_LOOP('',(#18086,#18087,#18088,#18089));
#6913=EDGE_LOOP('',(#18090,#18091,#18092,#18093));
#6914=EDGE_LOOP('',(#18094,#18095,#18096,#18097));
#6915=EDGE_LOOP('',(#18098,#18099,#18100,#18101));
#6916=EDGE_LOOP('',(#18102,#18103,#18104,#18105));
#6917=EDGE_LOOP('',(#18106,#18107,#18108,#18109));
#6918=EDGE_LOOP('',(#18110,#18111,#18112,#18113));
#6919=EDGE_LOOP('',(#18114,#18115,#18116,#18117));
#6920=EDGE_LOOP('',(#18118,#18119,#18120,#18121));
#6921=EDGE_LOOP('',(#18122,#18123,#18124,#18125));
#6922=EDGE_LOOP('',(#18126,#18127,#18128,#18129));
#6923=EDGE_LOOP('',(#18130,#18131,#18132,#18133));
#6924=EDGE_LOOP('',(#18134,#18135,#18136,#18137));
#6925=EDGE_LOOP('',(#18138,#18139,#18140,#18141));
#6926=EDGE_LOOP('',(#18142,#18143,#18144,#18145));
#6927=EDGE_LOOP('',(#18146,#18147,#18148,#18149));
#6928=EDGE_LOOP('',(#18150,#18151,#18152,#18153));
#6929=EDGE_LOOP('',(#18154,#18155,#18156,#18157));
#6930=EDGE_LOOP('',(#18158,#18159,#18160,#18161));
#6931=EDGE_LOOP('',(#18162,#18163,#18164,#18165));
#6932=EDGE_LOOP('',(#18166,#18167,#18168,#18169));
#6933=EDGE_LOOP('',(#18170,#18171,#18172,#18173));
#6934=EDGE_LOOP('',(#18174,#18175,#18176,#18177,#18178,#18179,#18180,#18181,
#18182,#18183,#18184,#18185,#18186,#18187,#18188,#18189,#18190,#18191,#18192,
#18193,#18194,#18195,#18196,#18197,#18198,#18199,#18200,#18201,#18202,#18203,
#18204,#18205,#18206,#18207));
#6935=EDGE_LOOP('',(#18208,#18209,#18210,#18211));
#6936=EDGE_LOOP('',(#18212,#18213,#18214,#18215));
#6937=EDGE_LOOP('',(#18216,#18217,#18218,#18219));
#6938=EDGE_LOOP('',(#18220,#18221,#18222,#18223));
#6939=EDGE_LOOP('',(#18224,#18225,#18226,#18227));
#6940=EDGE_LOOP('',(#18228,#18229,#18230,#18231));
#6941=EDGE_LOOP('',(#18232,#18233,#18234,#18235));
#6942=EDGE_LOOP('',(#18236,#18237,#18238,#18239));
#6943=EDGE_LOOP('',(#18240,#18241,#18242,#18243,#18244,#18245,#18246,#18247,
#18248,#18249,#18250,#18251,#18252,#18253,#18254,#18255,#18256,#18257,#18258,
#18259,#18260,#18261,#18262,#18263,#18264,#18265,#18266,#18267,#18268,#18269,
#18270,#18271,#18272,#18273));
#6944=EDGE_LOOP('',(#18274,#18275,#18276,#18277,#18278));
#6945=EDGE_LOOP('',(#18279,#18280,#18281,#18282,#18283,#18284));
#6946=EDGE_LOOP('',(#18285));
#6947=EDGE_LOOP('',(#18286));
#6948=EDGE_LOOP('',(#18287,#18288,#18289,#18290,#18291));
#6949=EDGE_LOOP('',(#18292));
#6950=EDGE_LOOP('',(#18293));
#6951=EDGE_LOOP('',(#18294,#18295,#18296,#18297));
#6952=EDGE_LOOP('',(#18298,#18299,#18300,#18301));
#6953=EDGE_LOOP('',(#18302,#18303,#18304,#18305));
#6954=EDGE_LOOP('',(#18306,#18307,#18308,#18309));
#6955=EDGE_LOOP('',(#18310,#18311,#18312,#18313));
#6956=EDGE_LOOP('',(#18314,#18315,#18316,#18317,#18318,#18319,#18320));
#6957=EDGE_LOOP('',(#18321,#18322,#18323,#18324));
#6958=EDGE_LOOP('',(#18325,#18326,#18327,#18328,#18329,#18330,#18331));
#6959=EDGE_LOOP('',(#18332,#18333,#18334,#18335));
#6960=EDGE_LOOP('',(#18336,#18337,#18338,#18339));
#6961=EDGE_LOOP('',(#18340,#18341,#18342,#18343,#18344));
#6962=EDGE_LOOP('',(#18345,#18346,#18347,#18348,#18349));
#6963=EDGE_LOOP('',(#18350));
#6964=EDGE_LOOP('',(#18351,#18352,#18353,#18354));
#6965=EDGE_LOOP('',(#18355,#18356,#18357,#18358));
#6966=EDGE_LOOP('',(#18359,#18360,#18361,#18362));
#6967=EDGE_LOOP('',(#18363,#18364,#18365,#18366));
#6968=EDGE_LOOP('',(#18367,#18368,#18369,#18370));
#6969=EDGE_LOOP('',(#18371,#18372,#18373,#18374,#18375));
#6970=EDGE_LOOP('',(#18376,#18377,#18378,#18379));
#6971=EDGE_LOOP('',(#18380,#18381,#18382,#18383));
#6972=EDGE_LOOP('',(#18384,#18385,#18386,#18387,#18388));
#6973=EDGE_LOOP('',(#18389));
#6974=EDGE_LOOP('',(#18390,#18391,#18392,#18393,#18394,#18395,#18396,#18397,
#18398,#18399,#18400,#18401,#18402,#18403,#18404,#18405));
#6975=EDGE_LOOP('',(#18406,#18407,#18408,#18409,#18410));
#6976=EDGE_LOOP('',(#18411,#18412,#18413,#18414));
#6977=EDGE_LOOP('',(#18415,#18416,#18417,#18418,#18419));
#6978=EDGE_LOOP('',(#18420,#18421,#18422,#18423,#18424));
#6979=EDGE_LOOP('',(#18425,#18426,#18427,#18428));
#6980=EDGE_LOOP('',(#18429,#18430,#18431,#18432,#18433));
#6981=EDGE_LOOP('',(#18434,#18435,#18436,#18437,#18438));
#6982=EDGE_LOOP('',(#18439,#18440,#18441,#18442,#18443));
#6983=EDGE_LOOP('',(#18444,#18445,#18446,#18447,#18448));
#6984=EDGE_LOOP('',(#18449,#18450,#18451,#18452,#18453));
#6985=EDGE_LOOP('',(#18454,#18455,#18456,#18457));
#6986=EDGE_LOOP('',(#18458,#18459,#18460,#18461));
#6987=EDGE_LOOP('',(#18462,#18463,#18464,#18465,#18466));
#6988=EDGE_LOOP('',(#18467,#18468,#18469,#18470,#18471,#18472,#18473,#18474,
#18475,#18476,#18477,#18478,#18479,#18480,#18481,#18482,#18483,#18484,#18485));
#6989=EDGE_LOOP('',(#18486,#18487,#18488,#18489));
#6990=EDGE_LOOP('',(#18490));
#6991=EDGE_LOOP('',(#18491));
#6992=EDGE_LOOP('',(#18492,#18493,#18494,#18495));
#6993=CIRCLE('',#19954,0.00772500000001);
#6994=CIRCLE('',#19955,0.000275);
#6995=CIRCLE('',#19956,0.00800000000001);
#6996=CIRCLE('',#19957,0.00800000000001);
#6997=CIRCLE('',#19959,0.00800000000001);
#6998=CIRCLE('',#19960,0.00800000000001);
#6999=CIRCLE('',#19962,0.00616666666667666);
#7000=CIRCLE('',#19964,0.000275);
#7001=CIRCLE('',#19965,0.00772500000001);
#7002=CIRCLE('',#19967,0.00616666666667666);
#7003=CIRCLE('',#19971,0.000250000000012414);
#7004=CIRCLE('',#19972,0.000250000000012414);
#7005=CIRCLE('',#19974,0.0134500000000135);
#7006=CIRCLE('',#19975,0.0134500000000135);
#7007=CIRCLE('',#19977,0.000250000000012074);
#7008=CIRCLE('',#19978,0.000250000000012074);
#7009=CIRCLE('',#19981,0.000250000000011423);
#7010=CIRCLE('',#19982,0.000250000000011423);
#7011=CIRCLE('',#19984,0.0134500000000139);
#7012=CIRCLE('',#19985,0.0134500000000139);
#7013=CIRCLE('',#19987,0.00025000000001101);
#7014=CIRCLE('',#19988,0.00025000000001101);
#7015=CIRCLE('',#19991,0.000250000000010237);
#7016=CIRCLE('',#19992,0.000250000000010237);
#7017=CIRCLE('',#19994,0.0134500000000141);
#7018=CIRCLE('',#19995,0.0134500000000141);
#7019=CIRCLE('',#19997,0.000250000000010237);
#7020=CIRCLE('',#19998,0.000250000000010237);
#7021=CIRCLE('',#20001,0.00025000000001101);
#7022=CIRCLE('',#20002,0.00025000000001101);
#7023=CIRCLE('',#20004,0.0134500000000141);
#7024=CIRCLE('',#20005,0.0134500000000141);
#7025=CIRCLE('',#20007,0.000250000000011423);
#7026=CIRCLE('',#20008,0.000250000000011423);
#7027=CIRCLE('',#20011,0.000250000000012074);
#7028=CIRCLE('',#20012,0.000250000000012074);
#7029=CIRCLE('',#20014,0.0134500000000138);
#7030=CIRCLE('',#20015,0.0134500000000138);
#7031=CIRCLE('',#20017,0.000250000000012414);
#7032=CIRCLE('',#20018,0.000250000000012414);
#7033=CIRCLE('',#20025,0.0130000000000133);
#7034=CIRCLE('',#20026,0.0130000000000133);
#7035=CIRCLE('',#20028,0.0130000000000133);
#7036=CIRCLE('',#20029,0.0130000000000133);
#7037=CIRCLE('',#20031,0.0139000000000133);
#7038=CIRCLE('',#20032,0.0130000000000133);
#7039=CIRCLE('',#20033,0.0130000000000133);
#7040=CIRCLE('',#20034,0.0130000000000133);
#7041=CIRCLE('',#20035,0.0130000000000133);
#7042=CIRCLE('',#20037,0.0130000000000133);
#7043=CIRCLE('',#20039,0.0130000000000133);
#7044=CIRCLE('',#20042,0.0130000000000133);
#7045=CIRCLE('',#20044,0.0139000000000133);
#7046=CIRCLE('',#20047,0.0130000000000133);
#7047=CIRCLE('',#20052,0.00450000000001);
#7048=CIRCLE('',#20053,0.00250000000001);
#7049=CIRCLE('',#20055,0.00250000000001);
#7050=CIRCLE('',#20057,0.00450000000001);
#7051=CIRCLE('',#20062,0.01465000000001);
#7052=CIRCLE('',#20065,0.01465000000001);
#7053=CIRCLE('',#20071,0.01390000000001);
#7054=CIRCLE('',#20079,0.01390000000001);
#7055=CIRCLE('',#20084,0.00150000000001414);
#7056=CIRCLE('',#20086,0.00150000000001414);
#7057=CIRCLE('',#20090,0.0146500000000141);
#7058=CIRCLE('',#20093,0.0146500000000141);
#7059=CIRCLE('',#20099,0.0139000000000141);
#7060=CIRCLE('',#20107,0.0139000000000141);
#7061=CIRCLE('',#20112,0.00150000000001);
#7062=CIRCLE('',#20114,0.00150000000001);
#7063=CIRCLE('',#20118,0.01465000000001);
#7064=CIRCLE('',#20121,0.01465000000001);
#7065=CIRCLE('',#20127,0.01390000000001);
#7066=CIRCLE('',#20135,0.01390000000001);
#7067=CIRCLE('',#20140,0.00150000000001414);
#7068=CIRCLE('',#20142,0.00150000000001414);
#7069=CIRCLE('',#20146,0.0146500000000141);
#7070=CIRCLE('',#20149,0.0146500000000141);
#7071=CIRCLE('',#20155,0.0139000000000141);
#7072=CIRCLE('',#20163,0.0139000000000141);
#7073=CIRCLE('',#20168,0.00150000000001);
#7074=CIRCLE('',#20170,0.00150000000001);
#7075=CIRCLE('',#20174,0.01465000000001);
#7076=CIRCLE('',#20177,0.01465000000001);
#7077=CIRCLE('',#20183,0.01390000000001);
#7078=CIRCLE('',#20191,0.01390000000001);
#7079=CIRCLE('',#20196,0.00150000000001414);
#7080=CIRCLE('',#20198,0.00150000000001414);
#7081=CIRCLE('',#20202,0.0146500000000141);
#7082=CIRCLE('',#20205,0.0146500000000141);
#7083=CIRCLE('',#20211,0.0139000000000141);
#7084=CIRCLE('',#20219,0.0139000000000141);
#7085=CIRCLE('',#20224,0.00150000000001);
#7086=CIRCLE('',#20226,0.00150000000001);
#7087=CIRCLE('',#20230,0.01465000000001);
#7088=CIRCLE('',#20233,0.01465000000001);
#7089=CIRCLE('',#20239,0.01390000000001);
#7090=CIRCLE('',#20247,0.01390000000001);
#7091=CIRCLE('',#20252,0.00150000000001414);
#7092=CIRCLE('',#20254,0.00150000000001414);
#7093=CIRCLE('',#20258,0.0146500000000141);
#7094=CIRCLE('',#20261,0.0146500000000141);
#7095=CIRCLE('',#20267,0.0139000000000141);
#7096=CIRCLE('',#20275,0.0139000000000141);
#7097=CIRCLE('',#20280,0.00150000000001);
#7098=CIRCLE('',#20282,0.00150000000001);
#7099=CIRCLE('',#20283,0.00150000000001);
#7100=CIRCLE('',#20284,0.00150000000001);
#7101=CIRCLE('',#20317,0.000500000000011295);
#7102=CIRCLE('',#20318,0.000500000000011295);
#7103=CIRCLE('',#20320,0.000500000000012369);
#7104=CIRCLE('',#20321,0.000500000000012369);
#7105=CIRCLE('',#20323,0.000500000000013203);
#7106=CIRCLE('',#20324,0.000500000000013203);
#7107=CIRCLE('',#20326,0.00050000000001378);
#7108=CIRCLE('',#20327,0.00050000000001378);
#7109=CIRCLE('',#20329,0.000500000000014088);
#7110=CIRCLE('',#20330,0.000500000000014088);
#7111=CIRCLE('',#20332,0.000500000000014123);
#7112=CIRCLE('',#20333,0.000500000000014123);
#7113=CIRCLE('',#20335,0.000500000000013882);
#7114=CIRCLE('',#20336,0.000500000000013882);
#7115=CIRCLE('',#20338,0.000500000000013372);
#7116=CIRCLE('',#20339,0.000500000000013372);
#7117=CIRCLE('',#20341,0.000500000000012601);
#7118=CIRCLE('',#20342,0.000500000000012601);
#7119=CIRCLE('',#20344,0.000500000000011585);
#7120=CIRCLE('',#20345,0.000500000000011585);
#7121=CIRCLE('',#20347,0.000500000000010343);
#7122=CIRCLE('',#20348,0.000500000000010343);
#7123=CIRCLE('',#20350,0.000500000000010991);
#7124=CIRCLE('',#20351,0.000500000000010991);
#7125=CIRCLE('',#20353,0.000500000000012122);
#7126=CIRCLE('',#20354,0.000500000000012122);
#7127=CIRCLE('',#20356,0.000500000000013018);
#7128=CIRCLE('',#20357,0.000500000000013018);
#7129=CIRCLE('',#20359,0.00050000000001366);
#7130=CIRCLE('',#20360,0.00050000000001366);
#7131=CIRCLE('',#20362,0.000500000000014037);
#7132=CIRCLE('',#20363,0.000500000000014037);
#7133=CIRCLE('',#20365,0.00050000000001414);
#7134=CIRCLE('',#20366,0.00050000000001414);
#7135=CIRCLE('',#20368,0.000500000000013968);
#7136=CIRCLE('',#20369,0.000500000000013968);
#7137=CIRCLE('',#20371,0.000500000000013524);
#7138=CIRCLE('',#20372,0.000500000000013524);
#7139=CIRCLE('',#20374,0.000500000000012817);
#7140=CIRCLE('',#20375,0.000500000000012817);
#7141=CIRCLE('',#20377,0.000500000000011861);
#7142=CIRCLE('',#20378,0.000500000000011861);
#7143=CIRCLE('',#20380,0.000500000000010673);
#7144=CIRCLE('',#20381,0.000500000000010673);
#7145=CIRCLE('',#20383,0.000500000000010673);
#7146=CIRCLE('',#20384,0.000500000000010673);
#7147=CIRCLE('',#20386,0.000500000000011861);
#7148=CIRCLE('',#20387,0.000500000000011861);
#7149=CIRCLE('',#20389,0.000500000000012817);
#7150=CIRCLE('',#20390,0.000500000000012817);
#7151=CIRCLE('',#20392,0.000500000000013524);
#7152=CIRCLE('',#20393,0.000500000000013524);
#7153=CIRCLE('',#20395,0.000500000000013968);
#7154=CIRCLE('',#20396,0.000500000000013968);
#7155=CIRCLE('',#20398,0.00050000000001414);
#7156=CIRCLE('',#20399,0.00050000000001414);
#7157=CIRCLE('',#20401,0.000500000000014037);
#7158=CIRCLE('',#20402,0.000500000000014037);
#7159=CIRCLE('',#20404,0.00050000000001366);
#7160=CIRCLE('',#20405,0.00050000000001366);
#7161=CIRCLE('',#20407,0.000500000000013018);
#7162=CIRCLE('',#20408,0.000500000000013018);
#7163=CIRCLE('',#20410,0.000500000000012122);
#7164=CIRCLE('',#20411,0.000500000000012122);
#7165=CIRCLE('',#20413,0.000500000000010991);
#7166=CIRCLE('',#20414,0.000500000000010991);
#7167=CIRCLE('',#20416,0.000500000000010343);
#7168=CIRCLE('',#20417,0.000500000000010343);
#7169=CIRCLE('',#20419,0.000500000000011585);
#7170=CIRCLE('',#20420,0.000500000000011585);
#7171=CIRCLE('',#20422,0.000500000000012601);
#7172=CIRCLE('',#20423,0.000500000000012601);
#7173=CIRCLE('',#20425,0.000500000000013372);
#7174=CIRCLE('',#20426,0.000500000000013372);
#7175=CIRCLE('',#20428,0.000500000000013882);
#7176=CIRCLE('',#20429,0.000500000000013882);
#7177=CIRCLE('',#20431,0.000500000000014123);
#7178=CIRCLE('',#20432,0.000500000000014123);
#7179=CIRCLE('',#20434,0.000500000000014088);
#7180=CIRCLE('',#20435,0.000500000000014088);
#7181=CIRCLE('',#20437,0.00050000000001378);
#7182=CIRCLE('',#20438,0.00050000000001378);
#7183=CIRCLE('',#20440,0.000500000000013203);
#7184=CIRCLE('',#20441,0.000500000000013203);
#7185=CIRCLE('',#20443,0.000500000000012369);
#7186=CIRCLE('',#20444,0.000500000000012369);
#7187=CIRCLE('',#20446,0.000500000000011295);
#7188=CIRCLE('',#20447,0.000500000000011295);
#7189=CIRCLE('',#20449,0.01290000000001);
#7190=CIRCLE('',#20450,0.00050000000001);
#7191=CIRCLE('',#20451,0.01290000000001);
#7192=CIRCLE('',#20452,0.01290000000001);
#7193=CIRCLE('',#20453,0.01290000000001);
#7194=CIRCLE('',#20454,0.01290000000001);
#7195=CIRCLE('',#20455,0.01290000000001);
#7196=CIRCLE('',#20456,0.01290000000001);
#7197=CIRCLE('',#20457,0.01290000000001);
#7198=CIRCLE('',#20458,0.01290000000001);
#7199=CIRCLE('',#20459,0.01290000000001);
#7200=CIRCLE('',#20460,0.01290000000001);
#7201=CIRCLE('',#20461,0.01290000000001);
#7202=CIRCLE('',#20462,0.01290000000001);
#7203=CIRCLE('',#20463,0.01290000000001);
#7204=CIRCLE('',#20464,0.01290000000001);
#7205=CIRCLE('',#20465,0.01290000000001);
#7206=CIRCLE('',#20466,0.01290000000001);
#7207=CIRCLE('',#20467,0.01290000000001);
#7208=CIRCLE('',#20468,0.01290000000001);
#7209=CIRCLE('',#20469,0.01290000000001);
#7210=CIRCLE('',#20470,0.01290000000001);
#7211=CIRCLE('',#20471,0.01290000000001);
#7212=CIRCLE('',#20472,0.01290000000001);
#7213=CIRCLE('',#20473,0.01290000000001);
#7214=CIRCLE('',#20474,0.01290000000001);
#7215=CIRCLE('',#20475,0.01290000000001);
#7216=CIRCLE('',#20476,0.01290000000001);
#7217=CIRCLE('',#20477,0.01290000000001);
#7218=CIRCLE('',#20478,0.01290000000001);
#7219=CIRCLE('',#20479,0.01290000000001);
#7220=CIRCLE('',#20480,0.01290000000001);
#7221=CIRCLE('',#20481,0.01290000000001);
#7222=CIRCLE('',#20482,0.01290000000001);
#7223=CIRCLE('',#20483,0.01290000000001);
#7224=CIRCLE('',#20484,0.01290000000001);
#7225=CIRCLE('',#20485,0.01290000000001);
#7226=CIRCLE('',#20486,0.01290000000001);
#7227=CIRCLE('',#20487,0.01290000000001);
#7228=CIRCLE('',#20488,0.01290000000001);
#7229=CIRCLE('',#20489,0.01290000000001);
#7230=CIRCLE('',#20490,0.01290000000001);
#7231=CIRCLE('',#20491,0.01290000000001);
#7232=CIRCLE('',#20492,0.01290000000001);
#7233=CIRCLE('',#20493,0.01290000000001);
#7234=CIRCLE('',#20494,0.01290000000001);
#7235=CIRCLE('',#20495,0.00250000000001);
#7236=CIRCLE('',#20497,0.01290000000001);
#7237=CIRCLE('',#20499,0.01290000000001);
#7238=CIRCLE('',#20501,0.01290000000001);
#7239=CIRCLE('',#20503,0.01290000000001);
#7240=CIRCLE('',#20505,0.01290000000001);
#7241=CIRCLE('',#20507,0.01290000000001);
#7242=CIRCLE('',#20509,0.01290000000001);
#7243=CIRCLE('',#20511,0.01290000000001);
#7244=CIRCLE('',#20513,0.01290000000001);
#7245=CIRCLE('',#20515,0.01290000000001);
#7246=CIRCLE('',#20517,0.01290000000001);
#7247=CIRCLE('',#20519,0.01290000000001);
#7248=CIRCLE('',#20521,0.01290000000001);
#7249=CIRCLE('',#20523,0.01290000000001);
#7250=CIRCLE('',#20525,0.01290000000001);
#7251=CIRCLE('',#20527,0.01290000000001);
#7252=CIRCLE('',#20529,0.01290000000001);
#7253=CIRCLE('',#20531,0.01290000000001);
#7254=CIRCLE('',#20533,0.01290000000001);
#7255=CIRCLE('',#20535,0.01290000000001);
#7256=CIRCLE('',#20537,0.01290000000001);
#7257=CIRCLE('',#20539,0.01290000000001);
#7258=CIRCLE('',#20541,0.01290000000001);
#7259=CIRCLE('',#20543,0.01290000000001);
#7260=CIRCLE('',#20545,0.01290000000001);
#7261=CIRCLE('',#20547,0.01290000000001);
#7262=CIRCLE('',#20549,0.01290000000001);
#7263=CIRCLE('',#20551,0.01290000000001);
#7264=CIRCLE('',#20553,0.01290000000001);
#7265=CIRCLE('',#20555,0.01290000000001);
#7266=CIRCLE('',#20557,0.01290000000001);
#7267=CIRCLE('',#20559,0.01290000000001);
#7268=CIRCLE('',#20561,0.01290000000001);
#7269=CIRCLE('',#20563,0.01290000000001);
#7270=CIRCLE('',#20565,0.01290000000001);
#7271=CIRCLE('',#20567,0.01290000000001);
#7272=CIRCLE('',#20569,0.01290000000001);
#7273=CIRCLE('',#20571,0.01290000000001);
#7274=CIRCLE('',#20573,0.01290000000001);
#7275=CIRCLE('',#20575,0.01290000000001);
#7276=CIRCLE('',#20577,0.01290000000001);
#7277=CIRCLE('',#20579,0.01290000000001);
#7278=CIRCLE('',#20581,0.01290000000001);
#7279=CIRCLE('',#20583,0.01290000000001);
#7280=CIRCLE('',#20585,0.00050000000001);
#7281=CIRCLE('',#20587,0.01290000000001);
#7282=CIRCLE('',#20588,0.00250000000001);
#7283=CIRCLE('',#20595,0.00199999999998973);
#7284=CIRCLE('',#20599,0.0251250000000126);
#7285=CIRCLE('',#20601,0.0251250000000126);
#7286=CIRCLE('',#20602,0.0251250000000126);
#7287=CIRCLE('',#20605,0.00200000000001397);
#7288=CIRCLE('',#20610,0.00199999999998997);
#7289=CIRCLE('',#20614,0.0251250000000138);
#7290=CIRCLE('',#20616,0.0251250000000138);
#7291=CIRCLE('',#20617,0.0251250000000138);
#7292=CIRCLE('',#20620,0.00199999999999762);
#7293=CIRCLE('',#20625,0.00200000000001296);
#7294=CIRCLE('',#20629,0.0251250000000138);
#7295=CIRCLE('',#20631,0.0251250000000138);
#7296=CIRCLE('',#20632,0.0251250000000138);
#7297=CIRCLE('',#20640,0.00199999999998998);
#7298=CIRCLE('',#20643,0.0251250000000291);
#7299=CIRCLE('',#20644,0.0251250000000291);
#7300=CIRCLE('',#20646,0.0251250000000291);
#7301=CIRCLE('',#20650,0.00200000000000295);
#7302=CIRCLE('',#20652,0.00199999999998605);
#7303=CIRCLE('',#20659,0.00300000000001);
#7304=CIRCLE('',#20660,0.00325000000001);
#7305=CIRCLE('',#20661,0.00325000000001);
#7306=CIRCLE('',#20662,0.00300000000001);
#7307=CIRCLE('',#20666,0.00300000000001);
#7308=CIRCLE('',#20667,0.00325000000001);
#7309=CIRCLE('',#20668,0.00325000000001);
#7310=CIRCLE('',#20669,0.00300000000001);
#7311=CIRCLE('',#20673,0.00300000000001);
#7312=CIRCLE('',#20674,0.00325000000001);
#7313=CIRCLE('',#20675,0.00325000000001);
#7314=CIRCLE('',#20676,0.00300000000001);
#7315=CIRCLE('',#20682,0.00325000000001);
#7316=CIRCLE('',#20683,0.00325000000001);
#7317=CIRCLE('',#20684,0.00450000000001);
#7318=CIRCLE('',#20686,0.00300000000001);
#7319=CIRCLE('',#20688,0.00300000000001);
#7320=CIRCLE('',#20690,0.00300000000001);
#7321=CIRCLE('',#20691,0.00300000000001);
#7322=CIRCLE('',#20693,0.00300000000001);
#7323=CIRCLE('',#20695,0.00300000000001);
#7324=CIRCLE('',#20697,0.00200000000001414);
#7325=CIRCLE('',#20698,0.00200000000001414);
#7326=CIRCLE('',#20701,0.00200000000001);
#7327=CIRCLE('',#20702,0.00170000000001);
#7328=CIRCLE('',#20703,0.00170000000001);
#7329=CIRCLE('',#20704,0.00170000000001);
#7330=CIRCLE('',#20705,0.00170000000001);
#7331=CIRCLE('',#20707,0.00200000000001);
#7332=CIRCLE('',#20716,0.000500000000014142);
#7333=CIRCLE('',#20717,0.000500000000014142);
#7334=CIRCLE('',#20720,0.000500000000014142);
#7335=CIRCLE('',#20721,0.000500000000014142);
#7336=CIRCLE('',#20724,0.000500000000014142);
#7337=CIRCLE('',#20725,0.000500000000014142);
#7338=CIRCLE('',#20728,0.000500000000014142);
#7339=CIRCLE('',#20729,0.000500000000014142);
#7340=CIRCLE('',#20735,0.00450000000001);
#7341=CIRCLE('',#20739,0.00347964100814074);
#7342=CIRCLE('',#20740,0.00347964100814074);
#7343=CIRCLE('',#20743,0.00347964100814074);
#7344=CIRCLE('',#20744,0.00347964100814074);
#7345=CIRCLE('',#20747,0.00347964100814074);
#7346=CIRCLE('',#20748,0.00347964100814074);
#7347=CIRCLE('',#20753,0.00347964100814074);
#7348=CIRCLE('',#20754,0.00347964100814074);
#7349=CIRCLE('',#20759,0.01300000000001);
#7350=CIRCLE('',#20760,0.01275000000001);
#7351=CIRCLE('',#20762,0.00825000000001);
#7352=CIRCLE('',#20764,0.01300000000001);
#7353=CIRCLE('',#20766,0.00800000000001);
#7354=CIRCLE('',#20767,0.00800000000001);
#7355=CIRCLE('',#20769,0.00800000000001);
#7356=CIRCLE('',#20771,0.00170000000001);
#7357=CIRCLE('',#20774,0.00170000000001);
#7358=CIRCLE('',#20777,0.00170000000001);
#7359=CIRCLE('',#20780,0.00170000000001);
#7360=CIRCLE('',#20784,0.00600000000001);
#7361=CIRCLE('',#20785,0.00600000000001);
#7362=CIRCLE('',#20794,0.00772500000001);
#7363=CIRCLE('',#20795,0.000275);
#7364=CIRCLE('',#20796,0.00800000000001);
#7365=CIRCLE('',#20797,0.00800000000001);
#7366=CIRCLE('',#20799,0.00800000000001);
#7367=CIRCLE('',#20800,0.00800000000001);
#7368=CIRCLE('',#20802,0.00616666666667666);
#7369=CIRCLE('',#20804,0.000275);
#7370=CIRCLE('',#20805,0.00772500000001);
#7371=CIRCLE('',#20807,0.00616666666667666);
#7372=CIRCLE('',#20813,0.00050000000001);
#7373=CIRCLE('',#20814,0.00050000000001);
#7374=CIRCLE('',#20824,0.00050000000001);
#7375=CIRCLE('',#20826,0.00050000000001);
#7376=CIRCLE('',#20835,0.00425000000001401);
#7377=CIRCLE('',#20836,0.00425000000001401);
#7378=CIRCLE('',#20838,0.000585000000012771);
#7379=CIRCLE('',#20839,0.000585000000012771);
#7380=CIRCLE('',#20842,0.00195000000001316);
#7381=CIRCLE('',#20843,0.00195000000001316);
#7382=CIRCLE('',#20845,0.00011700000001);
#7383=CIRCLE('',#20846,0.00011700000001);
#7384=CIRCLE('',#20849,0.00046800000001);
#7385=CIRCLE('',#20850,0.00046800000001);
#7386=CIRCLE('',#20852,0.00312000000001353);
#7387=CIRCLE('',#20853,0.00312000000001353);
#7388=CIRCLE('',#20855,0.000312000000012182);
#7389=CIRCLE('',#20856,0.000312000000012182);
#7390=CIRCLE('',#20859,0.00039000000001);
#7391=CIRCLE('',#20860,0.00039000000001);
#7392=CIRCLE('',#20863,0.00031200000001);
#7393=CIRCLE('',#20864,0.00031200000001);
#7394=CIRCLE('',#20866,0.00312000000001219);
#7395=CIRCLE('',#20867,0.00312000000001219);
#7396=CIRCLE('',#20869,0.00046800000001353);
#7397=CIRCLE('',#20870,0.00046800000001353);
#7398=CIRCLE('',#20873,0.000117000000012679);
#7399=CIRCLE('',#20874,0.000117000000012679);
#7400=CIRCLE('',#20876,0.00195000000001268);
#7401=CIRCLE('',#20877,0.00195000000001268);
#7402=CIRCLE('',#20880,0.000585000000014012);
#7403=CIRCLE('',#20881,0.000585000000014012);
#7404=CIRCLE('',#20886,0.000250000000013569);
#7405=CIRCLE('',#20887,0.000250000000013569);
#7406=CIRCLE('',#20889,0.0134500000000125);
#7407=CIRCLE('',#20890,0.0134500000000125);
#7408=CIRCLE('',#20892,0.000250000000013744);
#7409=CIRCLE('',#20893,0.000250000000013744);
#7410=CIRCLE('',#20896,0.000250000000013973);
#7411=CIRCLE('',#20897,0.000250000000013973);
#7412=CIRCLE('',#20899,0.0134500000000115);
#7413=CIRCLE('',#20900,0.0134500000000115);
#7414=CIRCLE('',#20902,0.000250000000014062);
#7415=CIRCLE('',#20903,0.000250000000014062);
#7416=CIRCLE('',#20906,0.000250000000014138);
#7417=CIRCLE('',#20907,0.000250000000014138);
#7418=CIRCLE('',#20909,0.0134500000000103);
#7419=CIRCLE('',#20910,0.0134500000000103);
#7420=CIRCLE('',#20912,0.000250000000014138);
#7421=CIRCLE('',#20913,0.000250000000014138);
#7422=CIRCLE('',#20916,0.000250000000014062);
#7423=CIRCLE('',#20917,0.000250000000014062);
#7424=CIRCLE('',#20919,0.0134500000000109);
#7425=CIRCLE('',#20920,0.0134500000000109);
#7426=CIRCLE('',#20922,0.000250000000013973);
#7427=CIRCLE('',#20923,0.000250000000013973);
#7428=CIRCLE('',#20926,0.000250000000013744);
#7429=CIRCLE('',#20927,0.000250000000013744);
#7430=CIRCLE('',#20929,0.013450000000012);
#7431=CIRCLE('',#20930,0.013450000000012);
#7432=CIRCLE('',#20932,0.000250000000013569);
#7433=CIRCLE('',#20933,0.000250000000013569);
#7434=CIRCLE('',#20940,0.0130000000000128);
#7435=CIRCLE('',#20941,0.0130000000000128);
#7436=CIRCLE('',#20943,0.0130000000000128);
#7437=CIRCLE('',#20944,0.0130000000000128);
#7438=CIRCLE('',#20946,0.0139000000000128);
#7439=CIRCLE('',#20947,0.0130000000000128);
#7440=CIRCLE('',#20948,0.0130000000000128);
#7441=CIRCLE('',#20949,0.0130000000000128);
#7442=CIRCLE('',#20950,0.0130000000000128);
#7443=CIRCLE('',#20952,0.0130000000000128);
#7444=CIRCLE('',#20954,0.0130000000000128);
#7445=CIRCLE('',#20957,0.0130000000000128);
#7446=CIRCLE('',#20960,0.0139000000000128);
#7447=CIRCLE('',#20963,0.0130000000000128);
#7448=CIRCLE('',#20967,0.00200000000000295);
#7449=CIRCLE('',#20971,0.0251250000000291);
#7450=CIRCLE('',#20973,0.0251250000000291);
#7451=CIRCLE('',#20976,0.00200000000001397);
#7452=CIRCLE('',#20980,0.0251250000000126);
#7453=CIRCLE('',#20982,0.0251250000000126);
#7454=CIRCLE('',#20985,0.00199999999999762);
#7455=CIRCLE('',#20989,0.0251250000000138);
#7456=CIRCLE('',#20991,0.0251250000000138);
#7457=CIRCLE('',#20994,0.00199999999998605);
#7458=CIRCLE('',#20998,0.0251250000000138);
#7459=CIRCLE('',#21000,0.0251250000000138);
#7460=CIRCLE('',#21003,0.00199999999998998);
#7461=CIRCLE('',#21007,0.00199999999998973);
#7462=CIRCLE('',#21011,0.00199999999998997);
#7463=CIRCLE('',#21015,0.00200000000001296);
#7464=CIRCLE('',#21024,0.00122950000001);
#7465=CIRCLE('',#21025,0.00122950000001);
#7466=CIRCLE('',#21026,0.00122950000001);
#7467=CIRCLE('',#21027,0.00122950000001);
#7468=CIRCLE('',#21030,0.00122950000001);
#7469=CIRCLE('',#21031,0.00122950000001);
#7470=CIRCLE('',#21032,0.00122950000001);
#7471=CIRCLE('',#21033,0.00122950000001);
#7472=CIRCLE('',#21034,0.01090000000001);
#7473=CIRCLE('',#21048,0.01300000000001);
#7474=CIRCLE('',#21051,0.01090000000001);
#7475=CIRCLE('',#21052,0.01065000000001);
#7476=CIRCLE('',#21053,0.01090000000001);
#7477=CIRCLE('',#21055,0.00475000000001);
#7478=CIRCLE('',#21058,0.00450000000001);
#7479=CIRCLE('',#21059,0.00450000000001);
#7480=CIRCLE('',#21061,0.00450000000001);
#7481=CIRCLE('',#21063,0.00475000000001);
#7482=CIRCLE('',#21065,0.00600000000001);
#7483=CIRCLE('',#21067,0.01300000000001);
#7484=CIRCLE('',#21068,0.01275000000001);
#7485=CIRCLE('',#21070,0.00825000000001);
#7486=CIRCLE('',#21073,0.00800000000001);
#7487=CIRCLE('',#21074,0.00800000000001);
#7488=CIRCLE('',#21076,0.00800000000001);
#7489=CIRCLE('',#21082,0.00600000000001);
#7490=CIRCLE('',#21091,0.000250000000013569);
#7491=CIRCLE('',#21092,0.000250000000013569);
#7492=CIRCLE('',#21094,0.0134500000000125);
#7493=CIRCLE('',#21095,0.0134500000000125);
#7494=CIRCLE('',#21097,0.000250000000013744);
#7495=CIRCLE('',#21098,0.000250000000013744);
#7496=CIRCLE('',#21101,0.000250000000013973);
#7497=CIRCLE('',#21102,0.000250000000013973);
#7498=CIRCLE('',#21104,0.0134500000000115);
#7499=CIRCLE('',#21105,0.0134500000000115);
#7500=CIRCLE('',#21107,0.000250000000014062);
#7501=CIRCLE('',#21108,0.000250000000014062);
#7502=CIRCLE('',#21111,0.000250000000014138);
#7503=CIRCLE('',#21112,0.000250000000014138);
#7504=CIRCLE('',#21114,0.0134500000000103);
#7505=CIRCLE('',#21115,0.0134500000000103);
#7506=CIRCLE('',#21117,0.000250000000014138);
#7507=CIRCLE('',#21118,0.000250000000014138);
#7508=CIRCLE('',#21121,0.000250000000014062);
#7509=CIRCLE('',#21122,0.000250000000014062);
#7510=CIRCLE('',#21124,0.0134500000000109);
#7511=CIRCLE('',#21125,0.0134500000000109);
#7512=CIRCLE('',#21127,0.000250000000013973);
#7513=CIRCLE('',#21128,0.000250000000013973);
#7514=CIRCLE('',#21131,0.000250000000013744);
#7515=CIRCLE('',#21132,0.000250000000013744);
#7516=CIRCLE('',#21134,0.013450000000012);
#7517=CIRCLE('',#21135,0.013450000000012);
#7518=CIRCLE('',#21137,0.000250000000013569);
#7519=CIRCLE('',#21138,0.000250000000013569);
#7520=CIRCLE('',#21145,0.0130000000000128);
#7521=CIRCLE('',#21146,0.0130000000000128);
#7522=CIRCLE('',#21148,0.0130000000000128);
#7523=CIRCLE('',#21149,0.0130000000000128);
#7524=CIRCLE('',#21151,0.0139000000000128);
#7525=CIRCLE('',#21152,0.0130000000000128);
#7526=CIRCLE('',#21153,0.0130000000000128);
#7527=CIRCLE('',#21154,0.0130000000000128);
#7528=CIRCLE('',#21155,0.0130000000000128);
#7529=CIRCLE('',#21157,0.0130000000000128);
#7530=CIRCLE('',#21159,0.0130000000000128);
#7531=CIRCLE('',#21162,0.0130000000000128);
#7532=CIRCLE('',#21165,0.0139000000000128);
#7533=CIRCLE('',#21168,0.0130000000000128);
#7534=CIRCLE('',#21172,0.00250000000001);
#7535=CIRCLE('',#21173,0.00250000000001);
#7536=CIRCLE('',#21174,0.00200000000001);
#7537=CIRCLE('',#21176,0.00200000000001);
#7538=CIRCLE('',#21177,0.00250000000001);
#7539=CIRCLE('',#21179,0.00200000000001);
#7540=CIRCLE('',#21180,0.00200000000001);
#7541=CIRCLE('',#21182,0.00250000000001);
#7542=CIRCLE('',#21184,0.00250000000001);
#7543=CIRCLE('',#21186,0.00250000000001);
#7544=CIRCLE('',#21190,0.00250000000001);
#7545=CIRCLE('',#21191,0.00250000000001);
#7546=CIRCLE('',#21193,0.00200000000001);
#7547=CIRCLE('',#21203,0.01300000000001);
#7548=CIRCLE('',#21210,0.01300000000001);
#7549=CIRCLE('',#21217,0.00075000000001);
#7550=CIRCLE('',#21218,0.00075000000001);
#7551=CIRCLE('',#21220,0.00075000000001);
#7552=CIRCLE('',#21221,0.00075000000001);
#7553=CIRCLE('',#21223,0.00075000000001);
#7554=CIRCLE('',#21224,0.00075000000001);
#7555=CIRCLE('',#21226,0.00075000000001);
#7556=CIRCLE('',#21227,0.00075000000001);
#7557=CIRCLE('',#21229,0.00060000000001);
#7558=CIRCLE('',#21230,0.00060000000001);
#7559=CIRCLE('',#21232,0.00060000000001);
#7560=CIRCLE('',#21233,0.00060000000001);
#7561=CIRCLE('',#21235,0.00060000000001);
#7562=CIRCLE('',#21236,0.00060000000001);
#7563=CIRCLE('',#21238,0.00060000000001);
#7564=CIRCLE('',#21239,0.00060000000001);
#7565=CIRCLE('',#21241,0.00060000000001);
#7566=CIRCLE('',#21242,0.00060000000001);
#7567=CIRCLE('',#21244,0.00060000000001);
#7568=CIRCLE('',#21245,0.00060000000001);
#7569=CIRCLE('',#21254,0.01375000000001);
#7570=CIRCLE('',#21255,0.01375000000001);
#7571=CIRCLE('',#21264,0.00050000000001);
#7572=CIRCLE('',#21265,0.00050000000001);
#7573=CIRCLE('',#21274,0.000250000000012414);
#7574=CIRCLE('',#21275,0.000250000000012414);
#7575=CIRCLE('',#21277,0.0134500000000135);
#7576=CIRCLE('',#21278,0.0134500000000135);
#7577=CIRCLE('',#21280,0.000250000000012074);
#7578=CIRCLE('',#21281,0.000250000000012074);
#7579=CIRCLE('',#21284,0.000250000000011423);
#7580=CIRCLE('',#21285,0.000250000000011423);
#7581=CIRCLE('',#21287,0.0134500000000139);
#7582=CIRCLE('',#21288,0.0134500000000139);
#7583=CIRCLE('',#21290,0.00025000000001101);
#7584=CIRCLE('',#21291,0.00025000000001101);
#7585=CIRCLE('',#21294,0.000250000000010237);
#7586=CIRCLE('',#21295,0.000250000000010237);
#7587=CIRCLE('',#21297,0.0134500000000141);
#7588=CIRCLE('',#21298,0.0134500000000141);
#7589=CIRCLE('',#21300,0.000250000000010237);
#7590=CIRCLE('',#21301,0.000250000000010237);
#7591=CIRCLE('',#21304,0.00025000000001101);
#7592=CIRCLE('',#21305,0.00025000000001101);
#7593=CIRCLE('',#21307,0.0134500000000141);
#7594=CIRCLE('',#21308,0.0134500000000141);
#7595=CIRCLE('',#21310,0.000250000000011423);
#7596=CIRCLE('',#21311,0.000250000000011423);
#7597=CIRCLE('',#21314,0.000250000000012074);
#7598=CIRCLE('',#21315,0.000250000000012074);
#7599=CIRCLE('',#21317,0.0134500000000138);
#7600=CIRCLE('',#21318,0.0134500000000138);
#7601=CIRCLE('',#21320,0.000250000000012414);
#7602=CIRCLE('',#21321,0.000250000000012414);
#7603=CIRCLE('',#21328,0.0130000000000133);
#7604=CIRCLE('',#21329,0.0130000000000133);
#7605=CIRCLE('',#21331,0.0130000000000133);
#7606=CIRCLE('',#21332,0.0130000000000133);
#7607=CIRCLE('',#21334,0.0139000000000133);
#7608=CIRCLE('',#21335,0.0130000000000133);
#7609=CIRCLE('',#21336,0.0130000000000133);
#7610=CIRCLE('',#21337,0.0130000000000133);
#7611=CIRCLE('',#21338,0.0130000000000133);
#7612=CIRCLE('',#21340,0.0130000000000133);
#7613=CIRCLE('',#21342,0.0130000000000133);
#7614=CIRCLE('',#21345,0.0130000000000133);
#7615=CIRCLE('',#21347,0.0139000000000133);
#7616=CIRCLE('',#21350,0.0130000000000133);
#7617=CIRCLE('',#21355,0.00387500000001);
#7618=CIRCLE('',#21356,0.00250000000001);
#7619=CIRCLE('',#21358,0.00250000000001);
#7620=CIRCLE('',#21360,0.00387500000001);
#7621=CIRCLE('',#21366,0.00050000000001);
#7622=CIRCLE('',#21368,0.00050000000001);
#7623=CIRCLE('',#21376,0.000500000000011295);
#7624=CIRCLE('',#21377,0.000500000000011295);
#7625=CIRCLE('',#21379,0.000500000000012369);
#7626=CIRCLE('',#21380,0.000500000000012369);
#7627=CIRCLE('',#21382,0.000500000000013203);
#7628=CIRCLE('',#21383,0.000500000000013203);
#7629=CIRCLE('',#21385,0.00050000000001378);
#7630=CIRCLE('',#21386,0.00050000000001378);
#7631=CIRCLE('',#21388,0.000500000000014088);
#7632=CIRCLE('',#21389,0.000500000000014088);
#7633=CIRCLE('',#21391,0.000500000000014123);
#7634=CIRCLE('',#21392,0.000500000000014123);
#7635=CIRCLE('',#21394,0.000500000000013882);
#7636=CIRCLE('',#21395,0.000500000000013882);
#7637=CIRCLE('',#21397,0.000500000000013372);
#7638=CIRCLE('',#21398,0.000500000000013372);
#7639=CIRCLE('',#21400,0.000500000000012601);
#7640=CIRCLE('',#21401,0.000500000000012601);
#7641=CIRCLE('',#21403,0.000500000000011585);
#7642=CIRCLE('',#21404,0.000500000000011585);
#7643=CIRCLE('',#21406,0.000500000000010343);
#7644=CIRCLE('',#21407,0.000500000000010343);
#7645=CIRCLE('',#21409,0.000500000000010991);
#7646=CIRCLE('',#21410,0.000500000000010991);
#7647=CIRCLE('',#21412,0.000500000000012122);
#7648=CIRCLE('',#21413,0.000500000000012122);
#7649=CIRCLE('',#21415,0.000500000000013018);
#7650=CIRCLE('',#21416,0.000500000000013018);
#7651=CIRCLE('',#21418,0.00050000000001366);
#7652=CIRCLE('',#21419,0.00050000000001366);
#7653=CIRCLE('',#21421,0.000500000000014037);
#7654=CIRCLE('',#21422,0.000500000000014037);
#7655=CIRCLE('',#21424,0.00050000000001414);
#7656=CIRCLE('',#21425,0.00050000000001414);
#7657=CIRCLE('',#21427,0.000500000000013968);
#7658=CIRCLE('',#21428,0.000500000000013968);
#7659=CIRCLE('',#21430,0.000500000000013524);
#7660=CIRCLE('',#21431,0.000500000000013524);
#7661=CIRCLE('',#21433,0.000500000000012817);
#7662=CIRCLE('',#21434,0.000500000000012817);
#7663=CIRCLE('',#21436,0.000500000000011861);
#7664=CIRCLE('',#21437,0.000500000000011861);
#7665=CIRCLE('',#21439,0.000500000000010673);
#7666=CIRCLE('',#21440,0.000500000000010673);
#7667=CIRCLE('',#21442,0.000500000000010673);
#7668=CIRCLE('',#21443,0.000500000000010673);
#7669=CIRCLE('',#21445,0.000500000000011861);
#7670=CIRCLE('',#21446,0.000500000000011861);
#7671=CIRCLE('',#21448,0.000500000000012817);
#7672=CIRCLE('',#21449,0.000500000000012817);
#7673=CIRCLE('',#21451,0.000500000000013524);
#7674=CIRCLE('',#21452,0.000500000000013524);
#7675=CIRCLE('',#21454,0.000500000000013968);
#7676=CIRCLE('',#21455,0.000500000000013968);
#7677=CIRCLE('',#21457,0.00050000000001414);
#7678=CIRCLE('',#21458,0.00050000000001414);
#7679=CIRCLE('',#21460,0.000500000000014037);
#7680=CIRCLE('',#21461,0.000500000000014037);
#7681=CIRCLE('',#21463,0.00050000000001366);
#7682=CIRCLE('',#21464,0.00050000000001366);
#7683=CIRCLE('',#21466,0.000500000000013018);
#7684=CIRCLE('',#21467,0.000500000000013018);
#7685=CIRCLE('',#21469,0.000500000000012122);
#7686=CIRCLE('',#21470,0.000500000000012122);
#7687=CIRCLE('',#21472,0.000500000000010991);
#7688=CIRCLE('',#21473,0.000500000000010991);
#7689=CIRCLE('',#21475,0.000500000000010343);
#7690=CIRCLE('',#21476,0.000500000000010343);
#7691=CIRCLE('',#21478,0.000500000000011585);
#7692=CIRCLE('',#21479,0.000500000000011585);
#7693=CIRCLE('',#21481,0.000500000000012601);
#7694=CIRCLE('',#21482,0.000500000000012601);
#7695=CIRCLE('',#21484,0.000500000000013372);
#7696=CIRCLE('',#21485,0.000500000000013372);
#7697=CIRCLE('',#21487,0.000500000000013882);
#7698=CIRCLE('',#21488,0.000500000000013882);
#7699=CIRCLE('',#21490,0.000500000000014123);
#7700=CIRCLE('',#21491,0.000500000000014123);
#7701=CIRCLE('',#21493,0.000500000000014088);
#7702=CIRCLE('',#21494,0.000500000000014088);
#7703=CIRCLE('',#21496,0.00050000000001378);
#7704=CIRCLE('',#21497,0.00050000000001378);
#7705=CIRCLE('',#21499,0.000500000000013203);
#7706=CIRCLE('',#21500,0.000500000000013203);
#7707=CIRCLE('',#21502,0.000500000000012369);
#7708=CIRCLE('',#21503,0.000500000000012369);
#7709=CIRCLE('',#21505,0.000500000000011295);
#7710=CIRCLE('',#21506,0.000500000000011295);
#7711=CIRCLE('',#21508,0.01290000000001);
#7712=CIRCLE('',#21509,0.00050000000001);
#7713=CIRCLE('',#21510,0.01290000000001);
#7714=CIRCLE('',#21511,0.01290000000001);
#7715=CIRCLE('',#21512,0.01290000000001);
#7716=CIRCLE('',#21513,0.01290000000001);
#7717=CIRCLE('',#21514,0.01290000000001);
#7718=CIRCLE('',#21515,0.01290000000001);
#7719=CIRCLE('',#21516,0.01290000000001);
#7720=CIRCLE('',#21517,0.01290000000001);
#7721=CIRCLE('',#21518,0.01290000000001);
#7722=CIRCLE('',#21519,0.01290000000001);
#7723=CIRCLE('',#21520,0.01290000000001);
#7724=CIRCLE('',#21521,0.01290000000001);
#7725=CIRCLE('',#21522,0.01290000000001);
#7726=CIRCLE('',#21523,0.01290000000001);
#7727=CIRCLE('',#21524,0.01290000000001);
#7728=CIRCLE('',#21525,0.01290000000001);
#7729=CIRCLE('',#21526,0.01290000000001);
#7730=CIRCLE('',#21527,0.01290000000001);
#7731=CIRCLE('',#21528,0.01290000000001);
#7732=CIRCLE('',#21529,0.01290000000001);
#7733=CIRCLE('',#21530,0.01290000000001);
#7734=CIRCLE('',#21531,0.01290000000001);
#7735=CIRCLE('',#21532,0.01290000000001);
#7736=CIRCLE('',#21533,0.01290000000001);
#7737=CIRCLE('',#21534,0.01290000000001);
#7738=CIRCLE('',#21535,0.01290000000001);
#7739=CIRCLE('',#21536,0.01290000000001);
#7740=CIRCLE('',#21537,0.01290000000001);
#7741=CIRCLE('',#21538,0.01290000000001);
#7742=CIRCLE('',#21539,0.01290000000001);
#7743=CIRCLE('',#21540,0.01290000000001);
#7744=CIRCLE('',#21541,0.01290000000001);
#7745=CIRCLE('',#21542,0.01290000000001);
#7746=CIRCLE('',#21543,0.01290000000001);
#7747=CIRCLE('',#21544,0.01290000000001);
#7748=CIRCLE('',#21545,0.01290000000001);
#7749=CIRCLE('',#21546,0.01290000000001);
#7750=CIRCLE('',#21547,0.01290000000001);
#7751=CIRCLE('',#21548,0.01290000000001);
#7752=CIRCLE('',#21549,0.01290000000001);
#7753=CIRCLE('',#21550,0.01290000000001);
#7754=CIRCLE('',#21551,0.01290000000001);
#7755=CIRCLE('',#21552,0.01290000000001);
#7756=CIRCLE('',#21553,0.01290000000001);
#7757=CIRCLE('',#21554,0.00250000000001);
#7758=CIRCLE('',#21556,0.01290000000001);
#7759=CIRCLE('',#21558,0.01290000000001);
#7760=CIRCLE('',#21560,0.01290000000001);
#7761=CIRCLE('',#21562,0.01290000000001);
#7762=CIRCLE('',#21564,0.01290000000001);
#7763=CIRCLE('',#21566,0.01290000000001);
#7764=CIRCLE('',#21568,0.01290000000001);
#7765=CIRCLE('',#21570,0.01290000000001);
#7766=CIRCLE('',#21572,0.01290000000001);
#7767=CIRCLE('',#21574,0.01290000000001);
#7768=CIRCLE('',#21576,0.01290000000001);
#7769=CIRCLE('',#21578,0.01290000000001);
#7770=CIRCLE('',#21580,0.01290000000001);
#7771=CIRCLE('',#21582,0.01290000000001);
#7772=CIRCLE('',#21584,0.01290000000001);
#7773=CIRCLE('',#21586,0.01290000000001);
#7774=CIRCLE('',#21588,0.01290000000001);
#7775=CIRCLE('',#21590,0.01290000000001);
#7776=CIRCLE('',#21592,0.01290000000001);
#7777=CIRCLE('',#21594,0.01290000000001);
#7778=CIRCLE('',#21596,0.01290000000001);
#7779=CIRCLE('',#21598,0.01290000000001);
#7780=CIRCLE('',#21600,0.01290000000001);
#7781=CIRCLE('',#21602,0.01290000000001);
#7782=CIRCLE('',#21604,0.01290000000001);
#7783=CIRCLE('',#21606,0.01290000000001);
#7784=CIRCLE('',#21608,0.01290000000001);
#7785=CIRCLE('',#21610,0.01290000000001);
#7786=CIRCLE('',#21612,0.01290000000001);
#7787=CIRCLE('',#21614,0.01290000000001);
#7788=CIRCLE('',#21616,0.01290000000001);
#7789=CIRCLE('',#21618,0.01290000000001);
#7790=CIRCLE('',#21620,0.01290000000001);
#7791=CIRCLE('',#21622,0.01290000000001);
#7792=CIRCLE('',#21624,0.01290000000001);
#7793=CIRCLE('',#21626,0.01290000000001);
#7794=CIRCLE('',#21628,0.01290000000001);
#7795=CIRCLE('',#21630,0.01290000000001);
#7796=CIRCLE('',#21632,0.01290000000001);
#7797=CIRCLE('',#21634,0.01290000000001);
#7798=CIRCLE('',#21636,0.01290000000001);
#7799=CIRCLE('',#21638,0.01290000000001);
#7800=CIRCLE('',#21640,0.01290000000001);
#7801=CIRCLE('',#21642,0.01290000000001);
#7802=CIRCLE('',#21644,0.00050000000001);
#7803=CIRCLE('',#21646,0.01290000000001);
#7804=CIRCLE('',#21647,0.00250000000001);
#7805=CIRCLE('',#21652,0.00250000000001);
#7806=CIRCLE('',#21653,0.000275);
#7807=CIRCLE('',#21654,0.00277500000001);
#7808=CIRCLE('',#21655,0.00250000000001);
#7809=CIRCLE('',#21657,0.00250000000001);
#7810=CIRCLE('',#21658,0.00250000000001);
#7811=CIRCLE('',#21660,0.00433333333334334);
#7812=CIRCLE('',#21662,0.00277500000001);
#7813=CIRCLE('',#21663,0.000275);
#7814=CIRCLE('',#21665,0.00433333333334334);
#7815=CIRCLE('',#21669,0.000250000000013569);
#7816=CIRCLE('',#21670,0.000250000000013569);
#7817=CIRCLE('',#21672,0.0134500000000125);
#7818=CIRCLE('',#21673,0.0134500000000125);
#7819=CIRCLE('',#21675,0.000250000000013744);
#7820=CIRCLE('',#21676,0.000250000000013744);
#7821=CIRCLE('',#21679,0.000250000000013973);
#7822=CIRCLE('',#21680,0.000250000000013973);
#7823=CIRCLE('',#21682,0.0134500000000115);
#7824=CIRCLE('',#21683,0.0134500000000115);
#7825=CIRCLE('',#21685,0.000250000000014062);
#7826=CIRCLE('',#21686,0.000250000000014062);
#7827=CIRCLE('',#21689,0.000250000000014138);
#7828=CIRCLE('',#21690,0.000250000000014138);
#7829=CIRCLE('',#21692,0.0134500000000103);
#7830=CIRCLE('',#21693,0.0134500000000103);
#7831=CIRCLE('',#21695,0.000250000000014138);
#7832=CIRCLE('',#21696,0.000250000000014138);
#7833=CIRCLE('',#21699,0.000250000000014062);
#7834=CIRCLE('',#21700,0.000250000000014062);
#7835=CIRCLE('',#21702,0.0134500000000109);
#7836=CIRCLE('',#21703,0.0134500000000109);
#7837=CIRCLE('',#21705,0.000250000000013973);
#7838=CIRCLE('',#21706,0.000250000000013973);
#7839=CIRCLE('',#21709,0.000250000000013744);
#7840=CIRCLE('',#21710,0.000250000000013744);
#7841=CIRCLE('',#21712,0.013450000000012);
#7842=CIRCLE('',#21713,0.013450000000012);
#7843=CIRCLE('',#21715,0.000250000000013569);
#7844=CIRCLE('',#21716,0.000250000000013569);
#7845=CIRCLE('',#21723,0.0130000000000128);
#7846=CIRCLE('',#21724,0.0130000000000128);
#7847=CIRCLE('',#21726,0.0130000000000128);
#7848=CIRCLE('',#21727,0.0130000000000128);
#7849=CIRCLE('',#21729,0.0139000000000128);
#7850=CIRCLE('',#21730,0.0130000000000128);
#7851=CIRCLE('',#21731,0.0130000000000128);
#7852=CIRCLE('',#21732,0.0130000000000128);
#7853=CIRCLE('',#21733,0.0130000000000128);
#7854=CIRCLE('',#21735,0.0130000000000128);
#7855=CIRCLE('',#21737,0.0130000000000128);
#7856=CIRCLE('',#21740,0.0130000000000128);
#7857=CIRCLE('',#21743,0.0139000000000128);
#7858=CIRCLE('',#21746,0.0130000000000128);
#7859=CIRCLE('',#21753,0.00050000000001);
#7860=CIRCLE('',#21755,0.00050000000001);
#7861=CIRCLE('',#21762,0.00200000000001249);
#7862=CIRCLE('',#21763,0.00200000000001249);
#7863=CIRCLE('',#21766,0.00200000000001249);
#7864=CIRCLE('',#21767,0.00200000000001249);
#7865=CIRCLE('',#21769,0.0251250000000138);
#7866=CIRCLE('',#21770,0.0251250000000138);
#7867=CIRCLE('',#21772,0.00200000000001249);
#7868=CIRCLE('',#21773,0.00200000000001249);
#7869=CIRCLE('',#21776,0.00200000000001249);
#7870=CIRCLE('',#21777,0.00200000000001249);
#7871=CIRCLE('',#21779,0.0251250000000138);
#7872=CIRCLE('',#21780,0.0251250000000138);
#7873=CIRCLE('',#21782,0.00200000000001249);
#7874=CIRCLE('',#21783,0.00200000000001249);
#7875=CIRCLE('',#21786,0.00200000000001249);
#7876=CIRCLE('',#21787,0.00200000000001249);
#7877=CIRCLE('',#21789,0.0251250000000138);
#7878=CIRCLE('',#21790,0.0251250000000138);
#7879=CIRCLE('',#21792,0.00200000000001249);
#7880=CIRCLE('',#21793,0.00200000000001249);
#7881=CIRCLE('',#21796,0.00200000000001249);
#7882=CIRCLE('',#21797,0.00200000000001249);
#7883=CIRCLE('',#21799,0.0251250000000138);
#7884=CIRCLE('',#21800,0.00170000000001);
#7885=CIRCLE('',#21801,0.00170000000001);
#7886=CIRCLE('',#21802,0.00170000000001);
#7887=CIRCLE('',#21803,0.00170000000001);
#7888=CIRCLE('',#21805,0.0251250000000138);
#7889=CIRCLE('',#21807,0.00170000000001);
#7890=CIRCLE('',#21809,0.00170000000001);
#7891=CIRCLE('',#21811,0.00170000000001);
#7892=CIRCLE('',#21813,0.00170000000001);
#7893=CIRCLE('',#21825,0.000250000000013569);
#7894=CIRCLE('',#21826,0.000250000000013569);
#7895=CIRCLE('',#21828,0.0134500000000125);
#7896=CIRCLE('',#21829,0.0134500000000125);
#7897=CIRCLE('',#21831,0.000250000000013744);
#7898=CIRCLE('',#21832,0.000250000000013744);
#7899=CIRCLE('',#21835,0.000250000000013973);
#7900=CIRCLE('',#21836,0.000250000000013973);
#7901=CIRCLE('',#21838,0.0134500000000115);
#7902=CIRCLE('',#21839,0.0134500000000115);
#7903=CIRCLE('',#21841,0.000250000000014062);
#7904=CIRCLE('',#21842,0.000250000000014062);
#7905=CIRCLE('',#21845,0.000250000000014138);
#7906=CIRCLE('',#21846,0.000250000000014138);
#7907=CIRCLE('',#21848,0.0134500000000103);
#7908=CIRCLE('',#21849,0.0134500000000103);
#7909=CIRCLE('',#21851,0.000250000000014138);
#7910=CIRCLE('',#21852,0.000250000000014138);
#7911=CIRCLE('',#21855,0.000250000000014062);
#7912=CIRCLE('',#21856,0.000250000000014062);
#7913=CIRCLE('',#21858,0.0134500000000109);
#7914=CIRCLE('',#21859,0.0134500000000109);
#7915=CIRCLE('',#21861,0.000250000000013973);
#7916=CIRCLE('',#21862,0.000250000000013973);
#7917=CIRCLE('',#21865,0.000250000000013744);
#7918=CIRCLE('',#21866,0.000250000000013744);
#7919=CIRCLE('',#21868,0.013450000000012);
#7920=CIRCLE('',#21869,0.013450000000012);
#7921=CIRCLE('',#21871,0.000250000000013569);
#7922=CIRCLE('',#21872,0.000250000000013569);
#7923=CIRCLE('',#21879,0.0130000000000128);
#7924=CIRCLE('',#21880,0.0130000000000128);
#7925=CIRCLE('',#21882,0.0130000000000128);
#7926=CIRCLE('',#21883,0.0130000000000128);
#7927=CIRCLE('',#21885,0.0139000000000128);
#7928=CIRCLE('',#21886,0.0130000000000128);
#7929=CIRCLE('',#21887,0.0130000000000128);
#7930=CIRCLE('',#21888,0.0130000000000128);
#7931=CIRCLE('',#21889,0.0130000000000128);
#7932=CIRCLE('',#21891,0.0130000000000128);
#7933=CIRCLE('',#21893,0.0130000000000128);
#7934=CIRCLE('',#21896,0.0130000000000128);
#7935=CIRCLE('',#21898,0.0139000000000128);
#7936=CIRCLE('',#21901,0.0130000000000128);
#7937=CIRCLE('',#21961,0.00250000000001);
#7938=CIRCLE('',#21962,0.00250000000001);
#7939=CIRCLE('',#21964,0.01200000000001);
#7940=CIRCLE('',#21965,0.01200000000001);
#7941=CIRCLE('',#21970,0.000250000000012414);
#7942=CIRCLE('',#21971,0.000250000000012414);
#7943=CIRCLE('',#21973,0.0134500000000135);
#7944=CIRCLE('',#21974,0.0134500000000135);
#7945=CIRCLE('',#21976,0.000250000000012074);
#7946=CIRCLE('',#21977,0.000250000000012074);
#7947=CIRCLE('',#21980,0.000250000000011423);
#7948=CIRCLE('',#21981,0.000250000000011423);
#7949=CIRCLE('',#21983,0.0134500000000139);
#7950=CIRCLE('',#21984,0.0134500000000139);
#7951=CIRCLE('',#21986,0.00025000000001101);
#7952=CIRCLE('',#21987,0.00025000000001101);
#7953=CIRCLE('',#21990,0.000250000000010237);
#7954=CIRCLE('',#21991,0.000250000000010237);
#7955=CIRCLE('',#21993,0.0134500000000141);
#7956=CIRCLE('',#21994,0.0134500000000141);
#7957=CIRCLE('',#21996,0.000250000000010237);
#7958=CIRCLE('',#21997,0.000250000000010237);
#7959=CIRCLE('',#22000,0.00025000000001101);
#7960=CIRCLE('',#22001,0.00025000000001101);
#7961=CIRCLE('',#22003,0.0134500000000141);
#7962=CIRCLE('',#22004,0.0134500000000141);
#7963=CIRCLE('',#22006,0.000250000000011423);
#7964=CIRCLE('',#22007,0.000250000000011423);
#7965=CIRCLE('',#22010,0.000250000000012074);
#7966=CIRCLE('',#22011,0.000250000000012074);
#7967=CIRCLE('',#22013,0.0134500000000138);
#7968=CIRCLE('',#22014,0.0134500000000138);
#7969=CIRCLE('',#22016,0.000250000000012414);
#7970=CIRCLE('',#22017,0.000250000000012414);
#7971=CIRCLE('',#22024,0.0130000000000133);
#7972=CIRCLE('',#22025,0.0130000000000133);
#7973=CIRCLE('',#22027,0.0130000000000133);
#7974=CIRCLE('',#22028,0.0130000000000133);
#7975=CIRCLE('',#22030,0.0139000000000133);
#7976=CIRCLE('',#22031,0.0130000000000133);
#7977=CIRCLE('',#22032,0.0130000000000133);
#7978=CIRCLE('',#22033,0.0130000000000133);
#7979=CIRCLE('',#22034,0.0130000000000133);
#7980=CIRCLE('',#22036,0.0130000000000133);
#7981=CIRCLE('',#22038,0.0130000000000133);
#7982=CIRCLE('',#22041,0.0130000000000133);
#7983=CIRCLE('',#22044,0.0139000000000133);
#7984=CIRCLE('',#22047,0.0130000000000133);
#7985=CIRCLE('',#22051,0.000250000000012414);
#7986=CIRCLE('',#22052,0.000250000000012414);
#7987=CIRCLE('',#22054,0.0134500000000135);
#7988=CIRCLE('',#22055,0.0134500000000135);
#7989=CIRCLE('',#22057,0.000250000000012074);
#7990=CIRCLE('',#22058,0.000250000000012074);
#7991=CIRCLE('',#22061,0.000250000000011423);
#7992=CIRCLE('',#22062,0.000250000000011423);
#7993=CIRCLE('',#22064,0.0134500000000139);
#7994=CIRCLE('',#22065,0.0134500000000139);
#7995=CIRCLE('',#22067,0.00025000000001101);
#7996=CIRCLE('',#22068,0.00025000000001101);
#7997=CIRCLE('',#22071,0.000250000000010237);
#7998=CIRCLE('',#22072,0.000250000000010237);
#7999=CIRCLE('',#22074,0.0134500000000141);
#8000=CIRCLE('',#22075,0.0134500000000141);
#8001=CIRCLE('',#22077,0.000250000000010237);
#8002=CIRCLE('',#22078,0.000250000000010237);
#8003=CIRCLE('',#22081,0.00025000000001101);
#8004=CIRCLE('',#22082,0.00025000000001101);
#8005=CIRCLE('',#22084,0.0134500000000141);
#8006=CIRCLE('',#22085,0.0134500000000141);
#8007=CIRCLE('',#22087,0.000250000000011423);
#8008=CIRCLE('',#22088,0.000250000000011423);
#8009=CIRCLE('',#22091,0.000250000000012074);
#8010=CIRCLE('',#22092,0.000250000000012074);
#8011=CIRCLE('',#22094,0.0134500000000138);
#8012=CIRCLE('',#22095,0.0134500000000138);
#8013=CIRCLE('',#22097,0.000250000000012414);
#8014=CIRCLE('',#22098,0.000250000000012414);
#8015=CIRCLE('',#22105,0.0130000000000133);
#8016=CIRCLE('',#22106,0.0130000000000133);
#8017=CIRCLE('',#22108,0.0130000000000133);
#8018=CIRCLE('',#22109,0.0130000000000133);
#8019=CIRCLE('',#22111,0.0139000000000133);
#8020=CIRCLE('',#22112,0.0130000000000133);
#8021=CIRCLE('',#22113,0.0130000000000133);
#8022=CIRCLE('',#22114,0.0130000000000133);
#8023=CIRCLE('',#22115,0.0130000000000133);
#8024=CIRCLE('',#22117,0.0130000000000133);
#8025=CIRCLE('',#22119,0.0130000000000133);
#8026=CIRCLE('',#22122,0.0130000000000133);
#8027=CIRCLE('',#22125,0.0139000000000133);
#8028=CIRCLE('',#22128,0.0130000000000133);
#8029=CIRCLE('',#22132,0.00250000000001);
#8030=CIRCLE('',#22133,0.000275);
#8031=CIRCLE('',#22134,0.00277500000001);
#8032=CIRCLE('',#22135,0.00250000000001);
#8033=CIRCLE('',#22137,0.00250000000001);
#8034=CIRCLE('',#22138,0.00250000000001);
#8035=CIRCLE('',#22140,0.00433333333334334);
#8036=CIRCLE('',#22142,0.00277500000001);
#8037=CIRCLE('',#22143,0.000275);
#8038=CIRCLE('',#22145,0.00433333333334334);
#8039=CIRCLE('',#22151,0.00050000000001);
#8040=CIRCLE('',#22152,0.00050000000001);
#8041=CIRCLE('',#22161,0.00150000000001);
#8042=CIRCLE('',#22162,0.00119327500001);
#8043=CIRCLE('',#22163,0.00150000000001);
#8044=CIRCLE('',#22165,0.00150000000001);
#8045=CIRCLE('',#22168,0.00136794617523955);
#8046=CIRCLE('',#22169,0.00147019793481599);
#8047=CIRCLE('',#22171,0.000819912302485476);
#8048=CIRCLE('',#22173,0.00136794617523955);
#8049=CIRCLE('',#22174,0.00147019793481599);
#8050=CIRCLE('',#22176,0.000819912302485476);
#8051=CIRCLE('',#22178,0.00136794617523955);
#8052=CIRCLE('',#22179,0.00147019793481599);
#8053=CIRCLE('',#22181,0.000819912302485476);
#8054=CIRCLE('',#22182,0.000819912302485476);
#8055=CIRCLE('',#22184,0.00136794617523955);
#8056=CIRCLE('',#22185,0.00147019793481599);
#8057=CIRCLE('',#22187,0.000819912302485476);
#8058=CIRCLE('',#22189,0.0027642230121603);
#8059=CIRCLE('',#22190,0.001);
#8060=CIRCLE('',#22191,0.002206040231424);
#8061=CIRCLE('',#22192,0.0027642230121603);
#8062=CIRCLE('',#22194,0.0049973967301825);
#8063=CIRCLE('',#22195,0.0049973967301825);
#8064=CIRCLE('',#22196,0.0049973967301825);
#8065=CIRCLE('',#22197,0.0049973967301825);
#8066=CIRCLE('',#22198,0.0049973967301825);
#8067=CIRCLE('',#22199,0.0049973967301825);
#8068=CIRCLE('',#22200,0.0049973967301825);
#8069=CIRCLE('',#22201,0.0049973967301825);
#8070=CIRCLE('',#22203,0.00280000000001);
#8071=CIRCLE('',#22218,0.00136468500001);
#8072=CIRCLE('',#22219,0.00136468500001);
#8073=VERTEX_POINT('',#28474);
#8074=VERTEX_POINT('',#28476);
#8075=VERTEX_POINT('',#28478);
#8076=VERTEX_POINT('',#28482);
#8077=VERTEX_POINT('',#28484);
#8078=VERTEX_POINT('',#28488);
#8079=VERTEX_POINT('',#28491);
#8080=VERTEX_POINT('',#28495);
#8081=VERTEX_POINT('',#28501);
#8082=VERTEX_POINT('',#28502);
#8083=VERTEX_POINT('',#28504);
#8084=VERTEX_POINT('',#28506);
#8085=VERTEX_POINT('',#28510);
#8086=VERTEX_POINT('',#28512);
#8087=VERTEX_POINT('',#28516);
#8088=VERTEX_POINT('',#28518);
#8089=VERTEX_POINT('',#28522);
#8090=VERTEX_POINT('',#28524);
#8091=VERTEX_POINT('',#28528);
#8092=VERTEX_POINT('',#28529);
#8093=VERTEX_POINT('',#28531);
#8094=VERTEX_POINT('',#28533);
#8095=VERTEX_POINT('',#28537);
#8096=VERTEX_POINT('',#28539);
#8097=VERTEX_POINT('',#28543);
#8098=VERTEX_POINT('',#28545);
#8099=VERTEX_POINT('',#28549);
#8100=VERTEX_POINT('',#28551);
#8101=VERTEX_POINT('',#28555);
#8102=VERTEX_POINT('',#28556);
#8103=VERTEX_POINT('',#28558);
#8104=VERTEX_POINT('',#28560);
#8105=VERTEX_POINT('',#28564);
#8106=VERTEX_POINT('',#28566);
#8107=VERTEX_POINT('',#28570);
#8108=VERTEX_POINT('',#28572);
#8109=VERTEX_POINT('',#28576);
#8110=VERTEX_POINT('',#28578);
#8111=VERTEX_POINT('',#28582);
#8112=VERTEX_POINT('',#28583);
#8113=VERTEX_POINT('',#28585);
#8114=VERTEX_POINT('',#28587);
#8115=VERTEX_POINT('',#28591);
#8116=VERTEX_POINT('',#28593);
#8117=VERTEX_POINT('',#28597);
#8118=VERTEX_POINT('',#28599);
#8119=VERTEX_POINT('',#28603);
#8120=VERTEX_POINT('',#28605);
#8121=VERTEX_POINT('',#28609);
#8122=VERTEX_POINT('',#28610);
#8123=VERTEX_POINT('',#28612);
#8124=VERTEX_POINT('',#28614);
#8125=VERTEX_POINT('',#28618);
#8126=VERTEX_POINT('',#28620);
#8127=VERTEX_POINT('',#28624);
#8128=VERTEX_POINT('',#28626);
#8129=VERTEX_POINT('',#28630);
#8130=VERTEX_POINT('',#28632);
#8131=VERTEX_POINT('',#28636);
#8132=VERTEX_POINT('',#28638);
#8133=VERTEX_POINT('',#28642);
#8134=VERTEX_POINT('',#28644);
#8135=VERTEX_POINT('',#28648);
#8136=VERTEX_POINT('',#28650);
#8137=VERTEX_POINT('',#28654);
#8138=VERTEX_POINT('',#28656);
#8139=VERTEX_POINT('',#28660);
#8140=VERTEX_POINT('',#28662);
#8141=VERTEX_POINT('',#28669);
#8142=VERTEX_POINT('',#28671);
#8143=VERTEX_POINT('',#28673);
#8144=VERTEX_POINT('',#28677);
#8145=VERTEX_POINT('',#28682);
#8146=VERTEX_POINT('',#28686);
#8147=VERTEX_POINT('',#28694);
#8148=VERTEX_POINT('',#28696);
#8149=VERTEX_POINT('',#28708);
#8150=VERTEX_POINT('',#28710);
#8151=VERTEX_POINT('',#28713);
#8152=VERTEX_POINT('',#28717);
#8153=VERTEX_POINT('',#28723);
#8154=VERTEX_POINT('',#28724);
#8155=VERTEX_POINT('',#28726);
#8156=VERTEX_POINT('',#28728);
#8157=VERTEX_POINT('',#28730);
#8158=VERTEX_POINT('',#28732);
#8159=VERTEX_POINT('',#28734);
#8160=VERTEX_POINT('',#28736);
#8161=VERTEX_POINT('',#28739);
#8162=VERTEX_POINT('',#28740);
#8163=VERTEX_POINT('',#28742);
#8164=VERTEX_POINT('',#28761);
#8165=VERTEX_POINT('',#28782);
#8166=VERTEX_POINT('',#28784);
#8167=VERTEX_POINT('',#28788);
#8168=VERTEX_POINT('',#28792);
#8169=VERTEX_POINT('',#28796);
#8170=VERTEX_POINT('',#28800);
#8171=VERTEX_POINT('',#28804);
#8172=VERTEX_POINT('',#28808);
#8173=VERTEX_POINT('',#28815);
#8174=VERTEX_POINT('',#28817);
#8175=VERTEX_POINT('',#28821);
#8176=VERTEX_POINT('',#28825);
#8177=VERTEX_POINT('',#28831);
#8178=VERTEX_POINT('',#28832);
#8179=VERTEX_POINT('',#28834);
#8180=VERTEX_POINT('',#28836);
#8181=VERTEX_POINT('',#28838);
#8182=VERTEX_POINT('',#28840);
#8183=VERTEX_POINT('',#28842);
#8184=VERTEX_POINT('',#28844);
#8185=VERTEX_POINT('',#28847);
#8186=VERTEX_POINT('',#28848);
#8187=VERTEX_POINT('',#28850);
#8188=VERTEX_POINT('',#28869);
#8189=VERTEX_POINT('',#28890);
#8190=VERTEX_POINT('',#28892);
#8191=VERTEX_POINT('',#28896);
#8192=VERTEX_POINT('',#28900);
#8193=VERTEX_POINT('',#28904);
#8194=VERTEX_POINT('',#28908);
#8195=VERTEX_POINT('',#28912);
#8196=VERTEX_POINT('',#28916);
#8197=VERTEX_POINT('',#28923);
#8198=VERTEX_POINT('',#28925);
#8199=VERTEX_POINT('',#28929);
#8200=VERTEX_POINT('',#28933);
#8201=VERTEX_POINT('',#28939);
#8202=VERTEX_POINT('',#28940);
#8203=VERTEX_POINT('',#28942);
#8204=VERTEX_POINT('',#28944);
#8205=VERTEX_POINT('',#28946);
#8206=VERTEX_POINT('',#28948);
#8207=VERTEX_POINT('',#28950);
#8208=VERTEX_POINT('',#28952);
#8209=VERTEX_POINT('',#28955);
#8210=VERTEX_POINT('',#28956);
#8211=VERTEX_POINT('',#28958);
#8212=VERTEX_POINT('',#28977);
#8213=VERTEX_POINT('',#28998);
#8214=VERTEX_POINT('',#29000);
#8215=VERTEX_POINT('',#29004);
#8216=VERTEX_POINT('',#29008);
#8217=VERTEX_POINT('',#29012);
#8218=VERTEX_POINT('',#29016);
#8219=VERTEX_POINT('',#29020);
#8220=VERTEX_POINT('',#29024);
#8221=VERTEX_POINT('',#29031);
#8222=VERTEX_POINT('',#29033);
#8223=VERTEX_POINT('',#29037);
#8224=VERTEX_POINT('',#29041);
#8225=VERTEX_POINT('',#29047);
#8226=VERTEX_POINT('',#29048);
#8227=VERTEX_POINT('',#29050);
#8228=VERTEX_POINT('',#29052);
#8229=VERTEX_POINT('',#29054);
#8230=VERTEX_POINT('',#29056);
#8231=VERTEX_POINT('',#29058);
#8232=VERTEX_POINT('',#29060);
#8233=VERTEX_POINT('',#29063);
#8234=VERTEX_POINT('',#29064);
#8235=VERTEX_POINT('',#29066);
#8236=VERTEX_POINT('',#29085);
#8237=VERTEX_POINT('',#29106);
#8238=VERTEX_POINT('',#29108);
#8239=VERTEX_POINT('',#29112);
#8240=VERTEX_POINT('',#29116);
#8241=VERTEX_POINT('',#29120);
#8242=VERTEX_POINT('',#29124);
#8243=VERTEX_POINT('',#29128);
#8244=VERTEX_POINT('',#29132);
#8245=VERTEX_POINT('',#29139);
#8246=VERTEX_POINT('',#29141);
#8247=VERTEX_POINT('',#29145);
#8248=VERTEX_POINT('',#29149);
#8249=VERTEX_POINT('',#29155);
#8250=VERTEX_POINT('',#29156);
#8251=VERTEX_POINT('',#29158);
#8252=VERTEX_POINT('',#29160);
#8253=VERTEX_POINT('',#29162);
#8254=VERTEX_POINT('',#29164);
#8255=VERTEX_POINT('',#29166);
#8256=VERTEX_POINT('',#29168);
#8257=VERTEX_POINT('',#29171);
#8258=VERTEX_POINT('',#29172);
#8259=VERTEX_POINT('',#29174);
#8260=VERTEX_POINT('',#29193);
#8261=VERTEX_POINT('',#29214);
#8262=VERTEX_POINT('',#29216);
#8263=VERTEX_POINT('',#29220);
#8264=VERTEX_POINT('',#29224);
#8265=VERTEX_POINT('',#29228);
#8266=VERTEX_POINT('',#29232);
#8267=VERTEX_POINT('',#29236);
#8268=VERTEX_POINT('',#29240);
#8269=VERTEX_POINT('',#29247);
#8270=VERTEX_POINT('',#29249);
#8271=VERTEX_POINT('',#29253);
#8272=VERTEX_POINT('',#29257);
#8273=VERTEX_POINT('',#29263);
#8274=VERTEX_POINT('',#29264);
#8275=VERTEX_POINT('',#29266);
#8276=VERTEX_POINT('',#29268);
#8277=VERTEX_POINT('',#29270);
#8278=VERTEX_POINT('',#29272);
#8279=VERTEX_POINT('',#29274);
#8280=VERTEX_POINT('',#29276);
#8281=VERTEX_POINT('',#29279);
#8282=VERTEX_POINT('',#29280);
#8283=VERTEX_POINT('',#29282);
#8284=VERTEX_POINT('',#29301);
#8285=VERTEX_POINT('',#29322);
#8286=VERTEX_POINT('',#29324);
#8287=VERTEX_POINT('',#29328);
#8288=VERTEX_POINT('',#29332);
#8289=VERTEX_POINT('',#29336);
#8290=VERTEX_POINT('',#29340);
#8291=VERTEX_POINT('',#29344);
#8292=VERTEX_POINT('',#29348);
#8293=VERTEX_POINT('',#29355);
#8294=VERTEX_POINT('',#29357);
#8295=VERTEX_POINT('',#29361);
#8296=VERTEX_POINT('',#29365);
#8297=VERTEX_POINT('',#29371);
#8298=VERTEX_POINT('',#29372);
#8299=VERTEX_POINT('',#29374);
#8300=VERTEX_POINT('',#29376);
#8301=VERTEX_POINT('',#29378);
#8302=VERTEX_POINT('',#29380);
#8303=VERTEX_POINT('',#29382);
#8304=VERTEX_POINT('',#29384);
#8305=VERTEX_POINT('',#29387);
#8306=VERTEX_POINT('',#29388);
#8307=VERTEX_POINT('',#29390);
#8308=VERTEX_POINT('',#29409);
#8309=VERTEX_POINT('',#29430);
#8310=VERTEX_POINT('',#29432);
#8311=VERTEX_POINT('',#29436);
#8312=VERTEX_POINT('',#29440);
#8313=VERTEX_POINT('',#29444);
#8314=VERTEX_POINT('',#29448);
#8315=VERTEX_POINT('',#29452);
#8316=VERTEX_POINT('',#29456);
#8317=VERTEX_POINT('',#29463);
#8318=VERTEX_POINT('',#29465);
#8319=VERTEX_POINT('',#29469);
#8320=VERTEX_POINT('',#29473);
#8321=VERTEX_POINT('',#29479);
#8322=VERTEX_POINT('',#29480);
#8323=VERTEX_POINT('',#29482);
#8324=VERTEX_POINT('',#29484);
#8325=VERTEX_POINT('',#29486);
#8326=VERTEX_POINT('',#29488);
#8327=VERTEX_POINT('',#29490);
#8328=VERTEX_POINT('',#29492);
#8329=VERTEX_POINT('',#29495);
#8330=VERTEX_POINT('',#29496);
#8331=VERTEX_POINT('',#29498);
#8332=VERTEX_POINT('',#29517);
#8333=VERTEX_POINT('',#29538);
#8334=VERTEX_POINT('',#29540);
#8335=VERTEX_POINT('',#29544);
#8336=VERTEX_POINT('',#29548);
#8337=VERTEX_POINT('',#29552);
#8338=VERTEX_POINT('',#29556);
#8339=VERTEX_POINT('',#29560);
#8340=VERTEX_POINT('',#29564);
#8341=VERTEX_POINT('',#29571);
#8342=VERTEX_POINT('',#29573);
#8343=VERTEX_POINT('',#29577);
#8344=VERTEX_POINT('',#29581);
#8345=VERTEX_POINT('',#29583);
#8346=VERTEX_POINT('',#29585);
#8347=VERTEX_POINT('',#29591);
#8348=VERTEX_POINT('',#29592);
#8349=VERTEX_POINT('',#29594);
#8350=VERTEX_POINT('',#29596);
#8351=VERTEX_POINT('',#29598);
#8352=VERTEX_POINT('',#29600);
#8353=VERTEX_POINT('',#29602);
#8354=VERTEX_POINT('',#29604);
#8355=VERTEX_POINT('',#29607);
#8356=VERTEX_POINT('',#29608);
#8357=VERTEX_POINT('',#29610);
#8358=VERTEX_POINT('',#29612);
#8359=VERTEX_POINT('',#29614);
#8360=VERTEX_POINT('',#29616);
#8361=VERTEX_POINT('',#29618);
#8362=VERTEX_POINT('',#29620);
#8363=VERTEX_POINT('',#29624);
#8364=VERTEX_POINT('',#29626);
#8365=VERTEX_POINT('',#29630);
#8366=VERTEX_POINT('',#29634);
#8367=VERTEX_POINT('',#29635);
#8368=VERTEX_POINT('',#29640);
#8369=VERTEX_POINT('',#29642);
#8370=VERTEX_POINT('',#29644);
#8371=VERTEX_POINT('',#29648);
#8372=VERTEX_POINT('',#29652);
#8373=VERTEX_POINT('',#29658);
#8374=VERTEX_POINT('',#29660);
#8375=VERTEX_POINT('',#29663);
#8376=VERTEX_POINT('',#29664);
#8377=VERTEX_POINT('',#29666);
#8378=VERTEX_POINT('',#29668);
#8379=VERTEX_POINT('',#29670);
#8380=VERTEX_POINT('',#29672);
#8381=VERTEX_POINT('',#29674);
#8382=VERTEX_POINT('',#29676);
#8383=VERTEX_POINT('',#29678);
#8384=VERTEX_POINT('',#29680);
#8385=VERTEX_POINT('',#29682);
#8386=VERTEX_POINT('',#29684);
#8387=VERTEX_POINT('',#29703);
#8388=VERTEX_POINT('',#29705);
#8389=VERTEX_POINT('',#29707);
#8390=VERTEX_POINT('',#29709);
#8391=VERTEX_POINT('',#29714);
#8392=VERTEX_POINT('',#29715);
#8393=VERTEX_POINT('',#29717);
#8394=VERTEX_POINT('',#29723);
#8395=VERTEX_POINT('',#29725);
#8396=VERTEX_POINT('',#29727);
#8397=VERTEX_POINT('',#29733);
#8398=VERTEX_POINT('',#29736);
#8399=VERTEX_POINT('',#29755);
#8400=VERTEX_POINT('',#29756);
#8401=VERTEX_POINT('',#29758);
#8402=VERTEX_POINT('',#29760);
#8403=VERTEX_POINT('',#29764);
#8404=VERTEX_POINT('',#29765);
#8405=VERTEX_POINT('',#29767);
#8406=VERTEX_POINT('',#29769);
#8407=VERTEX_POINT('',#29773);
#8408=VERTEX_POINT('',#29774);
#8409=VERTEX_POINT('',#29776);
#8410=VERTEX_POINT('',#29778);
#8411=VERTEX_POINT('',#29782);
#8412=VERTEX_POINT('',#29783);
#8413=VERTEX_POINT('',#29785);
#8414=VERTEX_POINT('',#29787);
#8415=VERTEX_POINT('',#29791);
#8416=VERTEX_POINT('',#29792);
#8417=VERTEX_POINT('',#29794);
#8418=VERTEX_POINT('',#29796);
#8419=VERTEX_POINT('',#29800);
#8420=VERTEX_POINT('',#29801);
#8421=VERTEX_POINT('',#29803);
#8422=VERTEX_POINT('',#29805);
#8423=VERTEX_POINT('',#29809);
#8424=VERTEX_POINT('',#29810);
#8425=VERTEX_POINT('',#29812);
#8426=VERTEX_POINT('',#29814);
#8427=VERTEX_POINT('',#29818);
#8428=VERTEX_POINT('',#29819);
#8429=VERTEX_POINT('',#29821);
#8430=VERTEX_POINT('',#29823);
#8431=VERTEX_POINT('',#29827);
#8432=VERTEX_POINT('',#29828);
#8433=VERTEX_POINT('',#29830);
#8434=VERTEX_POINT('',#29832);
#8435=VERTEX_POINT('',#29836);
#8436=VERTEX_POINT('',#29837);
#8437=VERTEX_POINT('',#29839);
#8438=VERTEX_POINT('',#29841);
#8439=VERTEX_POINT('',#29845);
#8440=VERTEX_POINT('',#29846);
#8441=VERTEX_POINT('',#29848);
#8442=VERTEX_POINT('',#29850);
#8443=VERTEX_POINT('',#29854);
#8444=VERTEX_POINT('',#29855);
#8445=VERTEX_POINT('',#29857);
#8446=VERTEX_POINT('',#29859);
#8447=VERTEX_POINT('',#29863);
#8448=VERTEX_POINT('',#29864);
#8449=VERTEX_POINT('',#29866);
#8450=VERTEX_POINT('',#29868);
#8451=VERTEX_POINT('',#29872);
#8452=VERTEX_POINT('',#29873);
#8453=VERTEX_POINT('',#29875);
#8454=VERTEX_POINT('',#29877);
#8455=VERTEX_POINT('',#29881);
#8456=VERTEX_POINT('',#29882);
#8457=VERTEX_POINT('',#29884);
#8458=VERTEX_POINT('',#29886);
#8459=VERTEX_POINT('',#29890);
#8460=VERTEX_POINT('',#29891);
#8461=VERTEX_POINT('',#29893);
#8462=VERTEX_POINT('',#29895);
#8463=VERTEX_POINT('',#29899);
#8464=VERTEX_POINT('',#29900);
#8465=VERTEX_POINT('',#29902);
#8466=VERTEX_POINT('',#29904);
#8467=VERTEX_POINT('',#29908);
#8468=VERTEX_POINT('',#29909);
#8469=VERTEX_POINT('',#29911);
#8470=VERTEX_POINT('',#29913);
#8471=VERTEX_POINT('',#29917);
#8472=VERTEX_POINT('',#29918);
#8473=VERTEX_POINT('',#29920);
#8474=VERTEX_POINT('',#29922);
#8475=VERTEX_POINT('',#29926);
#8476=VERTEX_POINT('',#29927);
#8477=VERTEX_POINT('',#29929);
#8478=VERTEX_POINT('',#29931);
#8479=VERTEX_POINT('',#29935);
#8480=VERTEX_POINT('',#29936);
#8481=VERTEX_POINT('',#29938);
#8482=VERTEX_POINT('',#29940);
#8483=VERTEX_POINT('',#29944);
#8484=VERTEX_POINT('',#29945);
#8485=VERTEX_POINT('',#29947);
#8486=VERTEX_POINT('',#29949);
#8487=VERTEX_POINT('',#29953);
#8488=VERTEX_POINT('',#29954);
#8489=VERTEX_POINT('',#29956);
#8490=VERTEX_POINT('',#29958);
#8491=VERTEX_POINT('',#29962);
#8492=VERTEX_POINT('',#29963);
#8493=VERTEX_POINT('',#29965);
#8494=VERTEX_POINT('',#29967);
#8495=VERTEX_POINT('',#29971);
#8496=VERTEX_POINT('',#29972);
#8497=VERTEX_POINT('',#29974);
#8498=VERTEX_POINT('',#29976);
#8499=VERTEX_POINT('',#29980);
#8500=VERTEX_POINT('',#29981);
#8501=VERTEX_POINT('',#29983);
#8502=VERTEX_POINT('',#29985);
#8503=VERTEX_POINT('',#29989);
#8504=VERTEX_POINT('',#29990);
#8505=VERTEX_POINT('',#29992);
#8506=VERTEX_POINT('',#29994);
#8507=VERTEX_POINT('',#29998);
#8508=VERTEX_POINT('',#29999);
#8509=VERTEX_POINT('',#30001);
#8510=VERTEX_POINT('',#30003);
#8511=VERTEX_POINT('',#30007);
#8512=VERTEX_POINT('',#30008);
#8513=VERTEX_POINT('',#30010);
#8514=VERTEX_POINT('',#30012);
#8515=VERTEX_POINT('',#30016);
#8516=VERTEX_POINT('',#30017);
#8517=VERTEX_POINT('',#30019);
#8518=VERTEX_POINT('',#30021);
#8519=VERTEX_POINT('',#30025);
#8520=VERTEX_POINT('',#30026);
#8521=VERTEX_POINT('',#30028);
#8522=VERTEX_POINT('',#30030);
#8523=VERTEX_POINT('',#30034);
#8524=VERTEX_POINT('',#30035);
#8525=VERTEX_POINT('',#30037);
#8526=VERTEX_POINT('',#30039);
#8527=VERTEX_POINT('',#30043);
#8528=VERTEX_POINT('',#30044);
#8529=VERTEX_POINT('',#30046);
#8530=VERTEX_POINT('',#30048);
#8531=VERTEX_POINT('',#30052);
#8532=VERTEX_POINT('',#30053);
#8533=VERTEX_POINT('',#30055);
#8534=VERTEX_POINT('',#30057);
#8535=VERTEX_POINT('',#30061);
#8536=VERTEX_POINT('',#30062);
#8537=VERTEX_POINT('',#30064);
#8538=VERTEX_POINT('',#30066);
#8539=VERTEX_POINT('',#30070);
#8540=VERTEX_POINT('',#30071);
#8541=VERTEX_POINT('',#30073);
#8542=VERTEX_POINT('',#30075);
#8543=VERTEX_POINT('',#30079);
#8544=VERTEX_POINT('',#30080);
#8545=VERTEX_POINT('',#30082);
#8546=VERTEX_POINT('',#30084);
#8547=VERTEX_POINT('',#30088);
#8548=VERTEX_POINT('',#30089);
#8549=VERTEX_POINT('',#30091);
#8550=VERTEX_POINT('',#30093);
#8551=VERTEX_POINT('',#30097);
#8552=VERTEX_POINT('',#30098);
#8553=VERTEX_POINT('',#30100);
#8554=VERTEX_POINT('',#30102);
#8555=VERTEX_POINT('',#30106);
#8556=VERTEX_POINT('',#30107);
#8557=VERTEX_POINT('',#30109);
#8558=VERTEX_POINT('',#30111);
#8559=VERTEX_POINT('',#30115);
#8560=VERTEX_POINT('',#30116);
#8561=VERTEX_POINT('',#30118);
#8562=VERTEX_POINT('',#30120);
#8563=VERTEX_POINT('',#30124);
#8564=VERTEX_POINT('',#30125);
#8565=VERTEX_POINT('',#30127);
#8566=VERTEX_POINT('',#30129);
#8567=VERTEX_POINT('',#30133);
#8568=VERTEX_POINT('',#30134);
#8569=VERTEX_POINT('',#30136);
#8570=VERTEX_POINT('',#30138);
#8571=VERTEX_POINT('',#30142);
#8572=VERTEX_POINT('',#30143);
#8573=VERTEX_POINT('',#30145);
#8574=VERTEX_POINT('',#30147);
#8575=VERTEX_POINT('',#30151);
#8576=VERTEX_POINT('',#30153);
#8577=VERTEX_POINT('',#30199);
#8578=VERTEX_POINT('',#30202);
#8579=VERTEX_POINT('',#30206);
#8580=VERTEX_POINT('',#30297);
#8581=VERTEX_POINT('',#30304);
#8582=VERTEX_POINT('',#30305);
#8583=VERTEX_POINT('',#30307);
#8584=VERTEX_POINT('',#30309);
#8585=VERTEX_POINT('',#30313);
#8586=VERTEX_POINT('',#30315);
#8587=VERTEX_POINT('',#30317);
#8588=VERTEX_POINT('',#30321);
#8589=VERTEX_POINT('',#30323);
#8590=VERTEX_POINT('',#30325);
#8591=VERTEX_POINT('',#30327);
#8592=VERTEX_POINT('',#30329);
#8593=VERTEX_POINT('',#30331);
#8594=VERTEX_POINT('',#30340);
#8595=VERTEX_POINT('',#30342);
#8596=VERTEX_POINT('',#30344);
#8597=VERTEX_POINT('',#30348);
#8598=VERTEX_POINT('',#30350);
#8599=VERTEX_POINT('',#30354);
#8600=VERTEX_POINT('',#30356);
#8601=VERTEX_POINT('',#30358);
#8602=VERTEX_POINT('',#30362);
#8603=VERTEX_POINT('',#30364);
#8604=VERTEX_POINT('',#30366);
#8605=VERTEX_POINT('',#30368);
#8606=VERTEX_POINT('',#30370);
#8607=VERTEX_POINT('',#30372);
#8608=VERTEX_POINT('',#30381);
#8609=VERTEX_POINT('',#30383);
#8610=VERTEX_POINT('',#30385);
#8611=VERTEX_POINT('',#30389);
#8612=VERTEX_POINT('',#30391);
#8613=VERTEX_POINT('',#30395);
#8614=VERTEX_POINT('',#30397);
#8615=VERTEX_POINT('',#30399);
#8616=VERTEX_POINT('',#30403);
#8617=VERTEX_POINT('',#30405);
#8618=VERTEX_POINT('',#30407);
#8619=VERTEX_POINT('',#30409);
#8620=VERTEX_POINT('',#30411);
#8621=VERTEX_POINT('',#30413);
#8622=VERTEX_POINT('',#30422);
#8623=VERTEX_POINT('',#30423);
#8624=VERTEX_POINT('',#30425);
#8625=VERTEX_POINT('',#30427);
#8626=VERTEX_POINT('',#30431);
#8627=VERTEX_POINT('',#30432);
#8628=VERTEX_POINT('',#30434);
#8629=VERTEX_POINT('',#30436);
#8630=VERTEX_POINT('',#30440);
#8631=VERTEX_POINT('',#30442);
#8632=VERTEX_POINT('',#30444);
#8633=VERTEX_POINT('',#30448);
#8634=VERTEX_POINT('',#30449);
#8635=VERTEX_POINT('',#30451);
#8636=VERTEX_POINT('',#30453);
#8637=VERTEX_POINT('',#30457);
#8638=VERTEX_POINT('',#30458);
#8639=VERTEX_POINT('',#30461);
#8640=VERTEX_POINT('',#30465);
#8641=VERTEX_POINT('',#30466);
#8642=VERTEX_POINT('',#30468);
#8643=VERTEX_POINT('',#30470);
#8644=VERTEX_POINT('',#30477);
#8645=VERTEX_POINT('',#30480);
#8646=VERTEX_POINT('',#30484);
#8647=VERTEX_POINT('',#30489);
#8648=VERTEX_POINT('',#30491);
#8649=VERTEX_POINT('',#30493);
#8650=VERTEX_POINT('',#30497);
#8651=VERTEX_POINT('',#30499);
#8652=VERTEX_POINT('',#30503);
#8653=VERTEX_POINT('',#30505);
#8654=VERTEX_POINT('',#30507);
#8655=VERTEX_POINT('',#30513);
#8656=VERTEX_POINT('',#30514);
#8657=VERTEX_POINT('',#30516);
#8658=VERTEX_POINT('',#30526);
#8659=VERTEX_POINT('',#30527);
#8660=VERTEX_POINT('',#30529);
#8661=VERTEX_POINT('',#30539);
#8662=VERTEX_POINT('',#30540);
#8663=VERTEX_POINT('',#30542);
#8664=VERTEX_POINT('',#30548);
#8665=VERTEX_POINT('',#30550);
#8666=VERTEX_POINT('',#30554);
#8667=VERTEX_POINT('',#30556);
#8668=VERTEX_POINT('',#30560);
#8669=VERTEX_POINT('',#30565);
#8670=VERTEX_POINT('',#30567);
#8671=VERTEX_POINT('',#30572);
#8672=VERTEX_POINT('',#30574);
#8673=VERTEX_POINT('',#30577);
#8674=VERTEX_POINT('',#30580);
#8675=VERTEX_POINT('',#30583);
#8676=VERTEX_POINT('',#30587);
#8677=VERTEX_POINT('',#30591);
#8678=VERTEX_POINT('',#30592);
#8679=VERTEX_POINT('',#30597);
#8680=VERTEX_POINT('',#30601);
#8681=VERTEX_POINT('',#30605);
#8682=VERTEX_POINT('',#30606);
#8683=VERTEX_POINT('',#30608);
#8684=VERTEX_POINT('',#30610);
#8685=VERTEX_POINT('',#30614);
#8686=VERTEX_POINT('',#30619);
#8687=VERTEX_POINT('',#30621);
#8688=VERTEX_POINT('',#30623);
#8689=VERTEX_POINT('',#30625);
#8690=VERTEX_POINT('',#30627);
#8691=VERTEX_POINT('',#30629);
#8692=VERTEX_POINT('',#30631);
#8693=VERTEX_POINT('',#30633);
#8694=VERTEX_POINT('',#30636);
#8695=VERTEX_POINT('',#30638);
#8696=VERTEX_POINT('',#30640);
#8697=VERTEX_POINT('',#30642);
#8698=VERTEX_POINT('',#30645);
#8699=VERTEX_POINT('',#30647);
#8700=VERTEX_POINT('',#30651);
#8701=VERTEX_POINT('',#30653);
#8702=VERTEX_POINT('',#30655);
#8703=VERTEX_POINT('',#30657);
#8704=VERTEX_POINT('',#30659);
#8705=VERTEX_POINT('',#30669);
#8706=VERTEX_POINT('',#30673);
#8707=VERTEX_POINT('',#30679);
#8708=VERTEX_POINT('',#30681);
#8709=VERTEX_POINT('',#30685);
#8710=VERTEX_POINT('',#30686);
#8711=VERTEX_POINT('',#30688);
#8712=VERTEX_POINT('',#30690);
#8713=VERTEX_POINT('',#30694);
#8714=VERTEX_POINT('',#30696);
#8715=VERTEX_POINT('',#30700);
#8716=VERTEX_POINT('',#30702);
#8717=VERTEX_POINT('',#30706);
#8718=VERTEX_POINT('',#30708);
#8719=VERTEX_POINT('',#30712);
#8720=VERTEX_POINT('',#30714);
#8721=VERTEX_POINT('',#30718);
#8722=VERTEX_POINT('',#30720);
#8723=VERTEX_POINT('',#30724);
#8724=VERTEX_POINT('',#30726);
#8725=VERTEX_POINT('',#30737);
#8726=VERTEX_POINT('',#30746);
#8727=VERTEX_POINT('',#30747);
#8728=VERTEX_POINT('',#30749);
#8729=VERTEX_POINT('',#30751);
#8730=VERTEX_POINT('',#30761);
#8731=VERTEX_POINT('',#30762);
#8732=VERTEX_POINT('',#30764);
#8733=VERTEX_POINT('',#30766);
#8734=VERTEX_POINT('',#30773);
#8735=VERTEX_POINT('',#30777);
#8736=VERTEX_POINT('',#30780);
#8737=VERTEX_POINT('',#30784);
#8738=VERTEX_POINT('',#30785);
#8739=VERTEX_POINT('',#30787);
#8740=VERTEX_POINT('',#30789);
#8741=VERTEX_POINT('',#30795);
#8742=VERTEX_POINT('',#30798);
#8743=VERTEX_POINT('',#30803);
#8744=VERTEX_POINT('',#30805);
#8745=VERTEX_POINT('',#30809);
#8746=VERTEX_POINT('',#30812);
#8747=VERTEX_POINT('',#30816);
#8748=VERTEX_POINT('',#30817);
#8749=VERTEX_POINT('',#30822);
#8750=VERTEX_POINT('',#30826);
#8751=VERTEX_POINT('',#30831);
#8752=VERTEX_POINT('',#30836);
#8753=VERTEX_POINT('',#30841);
#8754=VERTEX_POINT('',#30850);
#8755=VERTEX_POINT('',#30852);
#8756=VERTEX_POINT('',#30863);
#8757=VERTEX_POINT('',#30865);
#8758=VERTEX_POINT('',#30867);
#8759=VERTEX_POINT('',#30871);
#8760=VERTEX_POINT('',#30873);
#8761=VERTEX_POINT('',#30877);
#8762=VERTEX_POINT('',#30880);
#8763=VERTEX_POINT('',#30884);
#8764=VERTEX_POINT('',#30890);
#8765=VERTEX_POINT('',#30891);
#8766=VERTEX_POINT('',#30893);
#8767=VERTEX_POINT('',#30895);
#8768=VERTEX_POINT('',#30899);
#8769=VERTEX_POINT('',#30901);
#8770=VERTEX_POINT('',#30905);
#8771=VERTEX_POINT('',#30906);
#8772=VERTEX_POINT('',#30908);
#8773=VERTEX_POINT('',#30910);
#8774=VERTEX_POINT('',#30917);
#8775=VERTEX_POINT('',#30919);
#8776=VERTEX_POINT('',#30923);
#8777=VERTEX_POINT('',#30927);
#8778=VERTEX_POINT('',#30935);
#8779=VERTEX_POINT('',#30936);
#8780=VERTEX_POINT('',#30938);
#8781=VERTEX_POINT('',#30940);
#8782=VERTEX_POINT('',#30944);
#8783=VERTEX_POINT('',#30946);
#8784=VERTEX_POINT('',#30948);
#8785=VERTEX_POINT('',#30950);
#8786=VERTEX_POINT('',#30952);
#8787=VERTEX_POINT('',#30956);
#8788=VERTEX_POINT('',#30960);
#8789=VERTEX_POINT('',#30961);
#8790=VERTEX_POINT('',#30964);
#8791=VERTEX_POINT('',#30966);
#8792=VERTEX_POINT('',#30980);
#8793=VERTEX_POINT('',#30981);
#8794=VERTEX_POINT('',#30983);
#8795=VERTEX_POINT('',#30985);
#8796=VERTEX_POINT('',#30989);
#8797=VERTEX_POINT('',#30991);
#8798=VERTEX_POINT('',#30995);
#8799=VERTEX_POINT('',#30997);
#8800=VERTEX_POINT('',#31001);
#8801=VERTEX_POINT('',#31003);
#8802=VERTEX_POINT('',#31007);
#8803=VERTEX_POINT('',#31009);
#8804=VERTEX_POINT('',#31013);
#8805=VERTEX_POINT('',#31015);
#8806=VERTEX_POINT('',#31019);
#8807=VERTEX_POINT('',#31021);
#8808=VERTEX_POINT('',#31025);
#8809=VERTEX_POINT('',#31027);
#8810=VERTEX_POINT('',#31031);
#8811=VERTEX_POINT('',#31033);
#8812=VERTEX_POINT('',#31037);
#8813=VERTEX_POINT('',#31039);
#8814=VERTEX_POINT('',#31043);
#8815=VERTEX_POINT('',#31045);
#8816=VERTEX_POINT('',#31049);
#8817=VERTEX_POINT('',#31051);
#8818=VERTEX_POINT('',#31055);
#8819=VERTEX_POINT('',#31057);
#8820=VERTEX_POINT('',#31061);
#8821=VERTEX_POINT('',#31063);
#8822=VERTEX_POINT('',#31067);
#8823=VERTEX_POINT('',#31069);
#8824=VERTEX_POINT('',#31073);
#8825=VERTEX_POINT('',#31075);
#8826=VERTEX_POINT('',#31079);
#8827=VERTEX_POINT('',#31081);
#8828=VERTEX_POINT('',#31085);
#8829=VERTEX_POINT('',#31087);
#8830=VERTEX_POINT('',#31091);
#8831=VERTEX_POINT('',#31093);
#8832=VERTEX_POINT('',#31103);
#8833=VERTEX_POINT('',#31104);
#8834=VERTEX_POINT('',#31106);
#8835=VERTEX_POINT('',#31108);
#8836=VERTEX_POINT('',#31112);
#8837=VERTEX_POINT('',#31114);
#8838=VERTEX_POINT('',#31118);
#8839=VERTEX_POINT('',#31120);
#8840=VERTEX_POINT('',#31124);
#8841=VERTEX_POINT('',#31126);
#8842=VERTEX_POINT('',#31130);
#8843=VERTEX_POINT('',#31131);
#8844=VERTEX_POINT('',#31133);
#8845=VERTEX_POINT('',#31135);
#8846=VERTEX_POINT('',#31139);
#8847=VERTEX_POINT('',#31141);
#8848=VERTEX_POINT('',#31145);
#8849=VERTEX_POINT('',#31147);
#8850=VERTEX_POINT('',#31151);
#8851=VERTEX_POINT('',#31153);
#8852=VERTEX_POINT('',#31157);
#8853=VERTEX_POINT('',#31158);
#8854=VERTEX_POINT('',#31160);
#8855=VERTEX_POINT('',#31162);
#8856=VERTEX_POINT('',#31166);
#8857=VERTEX_POINT('',#31168);
#8858=VERTEX_POINT('',#31172);
#8859=VERTEX_POINT('',#31174);
#8860=VERTEX_POINT('',#31178);
#8861=VERTEX_POINT('',#31180);
#8862=VERTEX_POINT('',#31184);
#8863=VERTEX_POINT('',#31185);
#8864=VERTEX_POINT('',#31187);
#8865=VERTEX_POINT('',#31189);
#8866=VERTEX_POINT('',#31193);
#8867=VERTEX_POINT('',#31195);
#8868=VERTEX_POINT('',#31199);
#8869=VERTEX_POINT('',#31201);
#8870=VERTEX_POINT('',#31205);
#8871=VERTEX_POINT('',#31207);
#8872=VERTEX_POINT('',#31211);
#8873=VERTEX_POINT('',#31212);
#8874=VERTEX_POINT('',#31214);
#8875=VERTEX_POINT('',#31216);
#8876=VERTEX_POINT('',#31220);
#8877=VERTEX_POINT('',#31222);
#8878=VERTEX_POINT('',#31226);
#8879=VERTEX_POINT('',#31228);
#8880=VERTEX_POINT('',#31232);
#8881=VERTEX_POINT('',#31234);
#8882=VERTEX_POINT('',#31238);
#8883=VERTEX_POINT('',#31240);
#8884=VERTEX_POINT('',#31244);
#8885=VERTEX_POINT('',#31246);
#8886=VERTEX_POINT('',#31250);
#8887=VERTEX_POINT('',#31252);
#8888=VERTEX_POINT('',#31256);
#8889=VERTEX_POINT('',#31258);
#8890=VERTEX_POINT('',#31262);
#8891=VERTEX_POINT('',#31264);
#8892=VERTEX_POINT('',#31271);
#8893=VERTEX_POINT('',#31273);
#8894=VERTEX_POINT('',#31275);
#8895=VERTEX_POINT('',#31279);
#8896=VERTEX_POINT('',#31284);
#8897=VERTEX_POINT('',#31288);
#8898=VERTEX_POINT('',#31296);
#8899=VERTEX_POINT('',#31300);
#8900=VERTEX_POINT('',#31310);
#8901=VERTEX_POINT('',#31311);
#8902=VERTEX_POINT('',#31313);
#8903=VERTEX_POINT('',#31315);
#8904=VERTEX_POINT('',#31319);
#8905=VERTEX_POINT('',#31321);
#8906=VERTEX_POINT('',#31323);
#8907=VERTEX_POINT('',#31325);
#8908=VERTEX_POINT('',#31329);
#8909=VERTEX_POINT('',#31330);
#8910=VERTEX_POINT('',#31332);
#8911=VERTEX_POINT('',#31334);
#8912=VERTEX_POINT('',#31338);
#8913=VERTEX_POINT('',#31340);
#8914=VERTEX_POINT('',#31342);
#8915=VERTEX_POINT('',#31344);
#8916=VERTEX_POINT('',#31348);
#8917=VERTEX_POINT('',#31349);
#8918=VERTEX_POINT('',#31351);
#8919=VERTEX_POINT('',#31353);
#8920=VERTEX_POINT('',#31357);
#8921=VERTEX_POINT('',#31359);
#8922=VERTEX_POINT('',#31361);
#8923=VERTEX_POINT('',#31363);
#8924=VERTEX_POINT('',#31367);
#8925=VERTEX_POINT('',#31368);
#8926=VERTEX_POINT('',#31370);
#8927=VERTEX_POINT('',#31372);
#8928=VERTEX_POINT('',#31376);
#8929=VERTEX_POINT('',#31378);
#8930=VERTEX_POINT('',#31380);
#8931=VERTEX_POINT('',#31382);
#8932=VERTEX_POINT('',#31386);
#8933=VERTEX_POINT('',#31388);
#8934=VERTEX_POINT('',#31392);
#8935=VERTEX_POINT('',#31394);
#8936=VERTEX_POINT('',#31398);
#8937=VERTEX_POINT('',#31400);
#8938=VERTEX_POINT('',#31404);
#8939=VERTEX_POINT('',#31406);
#8940=VERTEX_POINT('',#31424);
#8941=VERTEX_POINT('',#31425);
#8942=VERTEX_POINT('',#31427);
#8943=VERTEX_POINT('',#31429);
#8944=VERTEX_POINT('',#31431);
#8945=VERTEX_POINT('',#31433);
#8946=VERTEX_POINT('',#31435);
#8947=VERTEX_POINT('',#31437);
#8948=VERTEX_POINT('',#31440);
#8949=VERTEX_POINT('',#31442);
#8950=VERTEX_POINT('',#31444);
#8951=VERTEX_POINT('',#31446);
#8952=VERTEX_POINT('',#31452);
#8953=VERTEX_POINT('',#31454);
#8954=VERTEX_POINT('',#31456);
#8955=VERTEX_POINT('',#31458);
#8956=VERTEX_POINT('',#31460);
#8957=VERTEX_POINT('',#31463);
#8958=VERTEX_POINT('',#31464);
#8959=VERTEX_POINT('',#31466);
#8960=VERTEX_POINT('',#31468);
#8961=VERTEX_POINT('',#31472);
#8962=VERTEX_POINT('',#31474);
#8963=VERTEX_POINT('',#31478);
#8964=VERTEX_POINT('',#31480);
#8965=VERTEX_POINT('',#31484);
#8966=VERTEX_POINT('',#31486);
#8967=VERTEX_POINT('',#31490);
#8968=VERTEX_POINT('',#31492);
#8969=VERTEX_POINT('',#31496);
#8970=VERTEX_POINT('',#31498);
#8971=VERTEX_POINT('',#31502);
#8972=VERTEX_POINT('',#31504);
#8973=VERTEX_POINT('',#31520);
#8974=VERTEX_POINT('',#31525);
#8975=VERTEX_POINT('',#31526);
#8976=VERTEX_POINT('',#31528);
#8977=VERTEX_POINT('',#31533);
#8978=VERTEX_POINT('',#31538);
#8979=VERTEX_POINT('',#31539);
#8980=VERTEX_POINT('',#31544);
#8981=VERTEX_POINT('',#31548);
#8982=VERTEX_POINT('',#31552);
#8983=VERTEX_POINT('',#31555);
#8984=VERTEX_POINT('',#31557);
#8985=VERTEX_POINT('',#31561);
#8986=VERTEX_POINT('',#31566);
#8987=VERTEX_POINT('',#31567);
#8988=VERTEX_POINT('',#31572);
#8989=VERTEX_POINT('',#31584);
#8990=VERTEX_POINT('',#31598);
#8991=VERTEX_POINT('',#31599);
#8992=VERTEX_POINT('',#31601);
#8993=VERTEX_POINT('',#31603);
#8994=VERTEX_POINT('',#31607);
#8995=VERTEX_POINT('',#31609);
#8996=VERTEX_POINT('',#31613);
#8997=VERTEX_POINT('',#31615);
#8998=VERTEX_POINT('',#31619);
#8999=VERTEX_POINT('',#31621);
#9000=VERTEX_POINT('',#31625);
#9001=VERTEX_POINT('',#31626);
#9002=VERTEX_POINT('',#31628);
#9003=VERTEX_POINT('',#31630);
#9004=VERTEX_POINT('',#31634);
#9005=VERTEX_POINT('',#31636);
#9006=VERTEX_POINT('',#31640);
#9007=VERTEX_POINT('',#31642);
#9008=VERTEX_POINT('',#31646);
#9009=VERTEX_POINT('',#31648);
#9010=VERTEX_POINT('',#31652);
#9011=VERTEX_POINT('',#31653);
#9012=VERTEX_POINT('',#31655);
#9013=VERTEX_POINT('',#31657);
#9014=VERTEX_POINT('',#31661);
#9015=VERTEX_POINT('',#31663);
#9016=VERTEX_POINT('',#31667);
#9017=VERTEX_POINT('',#31669);
#9018=VERTEX_POINT('',#31673);
#9019=VERTEX_POINT('',#31675);
#9020=VERTEX_POINT('',#31679);
#9021=VERTEX_POINT('',#31680);
#9022=VERTEX_POINT('',#31682);
#9023=VERTEX_POINT('',#31684);
#9024=VERTEX_POINT('',#31688);
#9025=VERTEX_POINT('',#31690);
#9026=VERTEX_POINT('',#31694);
#9027=VERTEX_POINT('',#31696);
#9028=VERTEX_POINT('',#31700);
#9029=VERTEX_POINT('',#31702);
#9030=VERTEX_POINT('',#31706);
#9031=VERTEX_POINT('',#31707);
#9032=VERTEX_POINT('',#31709);
#9033=VERTEX_POINT('',#31711);
#9034=VERTEX_POINT('',#31715);
#9035=VERTEX_POINT('',#31717);
#9036=VERTEX_POINT('',#31721);
#9037=VERTEX_POINT('',#31723);
#9038=VERTEX_POINT('',#31727);
#9039=VERTEX_POINT('',#31729);
#9040=VERTEX_POINT('',#31733);
#9041=VERTEX_POINT('',#31735);
#9042=VERTEX_POINT('',#31739);
#9043=VERTEX_POINT('',#31741);
#9044=VERTEX_POINT('',#31745);
#9045=VERTEX_POINT('',#31747);
#9046=VERTEX_POINT('',#31751);
#9047=VERTEX_POINT('',#31753);
#9048=VERTEX_POINT('',#31757);
#9049=VERTEX_POINT('',#31759);
#9050=VERTEX_POINT('',#31766);
#9051=VERTEX_POINT('',#31768);
#9052=VERTEX_POINT('',#31770);
#9053=VERTEX_POINT('',#31774);
#9054=VERTEX_POINT('',#31779);
#9055=VERTEX_POINT('',#31783);
#9056=VERTEX_POINT('',#31791);
#9057=VERTEX_POINT('',#31795);
#9058=VERTEX_POINT('',#31805);
#9059=VERTEX_POINT('',#31806);
#9060=VERTEX_POINT('',#31808);
#9061=VERTEX_POINT('',#31810);
#9062=VERTEX_POINT('',#31812);
#9063=VERTEX_POINT('',#31819);
#9064=VERTEX_POINT('',#31825);
#9065=VERTEX_POINT('',#31827);
#9066=VERTEX_POINT('',#31831);
#9067=VERTEX_POINT('',#31834);
#9068=VERTEX_POINT('',#31837);
#9069=VERTEX_POINT('',#31840);
#9070=VERTEX_POINT('',#31847);
#9071=VERTEX_POINT('',#31849);
#9072=VERTEX_POINT('',#31853);
#9073=VERTEX_POINT('',#31860);
#9074=VERTEX_POINT('',#31861);
#9075=VERTEX_POINT('',#31863);
#9076=VERTEX_POINT('',#31865);
#9077=VERTEX_POINT('',#31869);
#9078=VERTEX_POINT('',#31870);
#9079=VERTEX_POINT('',#31872);
#9080=VERTEX_POINT('',#31874);
#9081=VERTEX_POINT('',#31878);
#9082=VERTEX_POINT('',#31880);
#9083=VERTEX_POINT('',#31884);
#9084=VERTEX_POINT('',#31886);
#9085=VERTEX_POINT('',#31890);
#9086=VERTEX_POINT('',#31892);
#9087=VERTEX_POINT('',#31897);
#9088=VERTEX_POINT('',#31899);
#9089=VERTEX_POINT('',#31901);
#9090=VERTEX_POINT('',#31903);
#9091=VERTEX_POINT('',#31905);
#9092=VERTEX_POINT('',#31907);
#9093=VERTEX_POINT('',#31909);
#9094=VERTEX_POINT('',#31913);
#9095=VERTEX_POINT('',#31917);
#9096=VERTEX_POINT('',#31919);
#9097=VERTEX_POINT('',#31923);
#9098=VERTEX_POINT('',#31931);
#9099=VERTEX_POINT('',#31935);
#9100=VERTEX_POINT('',#31939);
#9101=VERTEX_POINT('',#31947);
#9102=VERTEX_POINT('',#31949);
#9103=VERTEX_POINT('',#31953);
#9104=VERTEX_POINT('',#31955);
#9105=VERTEX_POINT('',#31959);
#9106=VERTEX_POINT('',#31961);
#9107=VERTEX_POINT('',#31965);
#9108=VERTEX_POINT('',#31967);
#9109=VERTEX_POINT('',#31971);
#9110=VERTEX_POINT('',#31973);
#9111=VERTEX_POINT('',#31977);
#9112=VERTEX_POINT('',#31979);
#9113=VERTEX_POINT('',#31983);
#9114=VERTEX_POINT('',#31985);
#9115=VERTEX_POINT('',#31989);
#9116=VERTEX_POINT('',#31991);
#9117=VERTEX_POINT('',#31995);
#9118=VERTEX_POINT('',#31997);
#9119=VERTEX_POINT('',#32001);
#9120=VERTEX_POINT('',#32003);
#9121=VERTEX_POINT('',#32007);
#9122=VERTEX_POINT('',#32008);
#9123=VERTEX_POINT('',#32010);
#9124=VERTEX_POINT('',#32012);
#9125=VERTEX_POINT('',#32016);
#9126=VERTEX_POINT('',#32018);
#9127=VERTEX_POINT('',#32022);
#9128=VERTEX_POINT('',#32023);
#9129=VERTEX_POINT('',#32025);
#9130=VERTEX_POINT('',#32027);
#9131=VERTEX_POINT('',#32034);
#9132=VERTEX_POINT('',#32035);
#9133=VERTEX_POINT('',#32037);
#9134=VERTEX_POINT('',#32039);
#9135=VERTEX_POINT('',#32043);
#9136=VERTEX_POINT('',#32045);
#9137=VERTEX_POINT('',#32052);
#9138=VERTEX_POINT('',#32054);
#9139=VERTEX_POINT('',#32058);
#9140=VERTEX_POINT('',#32060);
#9141=VERTEX_POINT('',#32070);
#9142=VERTEX_POINT('',#32071);
#9143=VERTEX_POINT('',#32073);
#9144=VERTEX_POINT('',#32075);
#9145=VERTEX_POINT('',#32079);
#9146=VERTEX_POINT('',#32081);
#9147=VERTEX_POINT('',#32085);
#9148=VERTEX_POINT('',#32086);
#9149=VERTEX_POINT('',#32088);
#9150=VERTEX_POINT('',#32090);
#9151=VERTEX_POINT('',#32097);
#9152=VERTEX_POINT('',#32099);
#9153=VERTEX_POINT('',#32103);
#9154=VERTEX_POINT('',#32107);
#9155=VERTEX_POINT('',#32115);
#9156=VERTEX_POINT('',#32116);
#9157=VERTEX_POINT('',#32118);
#9158=VERTEX_POINT('',#32120);
#9159=VERTEX_POINT('',#32124);
#9160=VERTEX_POINT('',#32126);
#9161=VERTEX_POINT('',#32130);
#9162=VERTEX_POINT('',#32132);
#9163=VERTEX_POINT('',#32136);
#9164=VERTEX_POINT('',#32138);
#9165=VERTEX_POINT('',#32142);
#9166=VERTEX_POINT('',#32143);
#9167=VERTEX_POINT('',#32145);
#9168=VERTEX_POINT('',#32147);
#9169=VERTEX_POINT('',#32151);
#9170=VERTEX_POINT('',#32153);
#9171=VERTEX_POINT('',#32157);
#9172=VERTEX_POINT('',#32159);
#9173=VERTEX_POINT('',#32163);
#9174=VERTEX_POINT('',#32165);
#9175=VERTEX_POINT('',#32169);
#9176=VERTEX_POINT('',#32170);
#9177=VERTEX_POINT('',#32172);
#9178=VERTEX_POINT('',#32174);
#9179=VERTEX_POINT('',#32178);
#9180=VERTEX_POINT('',#32180);
#9181=VERTEX_POINT('',#32184);
#9182=VERTEX_POINT('',#32186);
#9183=VERTEX_POINT('',#32190);
#9184=VERTEX_POINT('',#32192);
#9185=VERTEX_POINT('',#32196);
#9186=VERTEX_POINT('',#32197);
#9187=VERTEX_POINT('',#32199);
#9188=VERTEX_POINT('',#32201);
#9189=VERTEX_POINT('',#32205);
#9190=VERTEX_POINT('',#32207);
#9191=VERTEX_POINT('',#32211);
#9192=VERTEX_POINT('',#32213);
#9193=VERTEX_POINT('',#32217);
#9194=VERTEX_POINT('',#32219);
#9195=VERTEX_POINT('',#32223);
#9196=VERTEX_POINT('',#32224);
#9197=VERTEX_POINT('',#32226);
#9198=VERTEX_POINT('',#32228);
#9199=VERTEX_POINT('',#32232);
#9200=VERTEX_POINT('',#32234);
#9201=VERTEX_POINT('',#32238);
#9202=VERTEX_POINT('',#32240);
#9203=VERTEX_POINT('',#32244);
#9204=VERTEX_POINT('',#32246);
#9205=VERTEX_POINT('',#32250);
#9206=VERTEX_POINT('',#32252);
#9207=VERTEX_POINT('',#32256);
#9208=VERTEX_POINT('',#32258);
#9209=VERTEX_POINT('',#32262);
#9210=VERTEX_POINT('',#32264);
#9211=VERTEX_POINT('',#32268);
#9212=VERTEX_POINT('',#32270);
#9213=VERTEX_POINT('',#32274);
#9214=VERTEX_POINT('',#32276);
#9215=VERTEX_POINT('',#32283);
#9216=VERTEX_POINT('',#32285);
#9217=VERTEX_POINT('',#32287);
#9218=VERTEX_POINT('',#32291);
#9219=VERTEX_POINT('',#32296);
#9220=VERTEX_POINT('',#32300);
#9221=VERTEX_POINT('',#32308);
#9222=VERTEX_POINT('',#32310);
#9223=VERTEX_POINT('',#32322);
#9224=VERTEX_POINT('',#32324);
#9225=VERTEX_POINT('',#32327);
#9226=VERTEX_POINT('',#32331);
#9227=VERTEX_POINT('',#32337);
#9228=VERTEX_POINT('',#32338);
#9229=VERTEX_POINT('',#32340);
#9230=VERTEX_POINT('',#32342);
#9231=VERTEX_POINT('',#32346);
#9232=VERTEX_POINT('',#32348);
#9233=VERTEX_POINT('',#32352);
#9234=VERTEX_POINT('',#32354);
#9235=VERTEX_POINT('',#32356);
#9236=VERTEX_POINT('',#32358);
#9237=VERTEX_POINT('',#32362);
#9238=VERTEX_POINT('',#32364);
#9239=VERTEX_POINT('',#32369);
#9240=VERTEX_POINT('',#32371);
#9241=VERTEX_POINT('',#32382);
#9242=VERTEX_POINT('',#32383);
#9243=VERTEX_POINT('',#32385);
#9244=VERTEX_POINT('',#32387);
#9245=VERTEX_POINT('',#32391);
#9246=VERTEX_POINT('',#32392);
#9247=VERTEX_POINT('',#32394);
#9248=VERTEX_POINT('',#32396);
#9249=VERTEX_POINT('',#32400);
#9250=VERTEX_POINT('',#32401);
#9251=VERTEX_POINT('',#32403);
#9252=VERTEX_POINT('',#32405);
#9253=VERTEX_POINT('',#32409);
#9254=VERTEX_POINT('',#32410);
#9255=VERTEX_POINT('',#32412);
#9256=VERTEX_POINT('',#32414);
#9257=VERTEX_POINT('',#32418);
#9258=VERTEX_POINT('',#32419);
#9259=VERTEX_POINT('',#32421);
#9260=VERTEX_POINT('',#32423);
#9261=VERTEX_POINT('',#32427);
#9262=VERTEX_POINT('',#32428);
#9263=VERTEX_POINT('',#32430);
#9264=VERTEX_POINT('',#32432);
#9265=VERTEX_POINT('',#32436);
#9266=VERTEX_POINT('',#32437);
#9267=VERTEX_POINT('',#32439);
#9268=VERTEX_POINT('',#32441);
#9269=VERTEX_POINT('',#32445);
#9270=VERTEX_POINT('',#32446);
#9271=VERTEX_POINT('',#32448);
#9272=VERTEX_POINT('',#32450);
#9273=VERTEX_POINT('',#32454);
#9274=VERTEX_POINT('',#32455);
#9275=VERTEX_POINT('',#32457);
#9276=VERTEX_POINT('',#32459);
#9277=VERTEX_POINT('',#32463);
#9278=VERTEX_POINT('',#32464);
#9279=VERTEX_POINT('',#32466);
#9280=VERTEX_POINT('',#32468);
#9281=VERTEX_POINT('',#32472);
#9282=VERTEX_POINT('',#32473);
#9283=VERTEX_POINT('',#32475);
#9284=VERTEX_POINT('',#32477);
#9285=VERTEX_POINT('',#32481);
#9286=VERTEX_POINT('',#32482);
#9287=VERTEX_POINT('',#32484);
#9288=VERTEX_POINT('',#32486);
#9289=VERTEX_POINT('',#32490);
#9290=VERTEX_POINT('',#32491);
#9291=VERTEX_POINT('',#32493);
#9292=VERTEX_POINT('',#32495);
#9293=VERTEX_POINT('',#32499);
#9294=VERTEX_POINT('',#32500);
#9295=VERTEX_POINT('',#32502);
#9296=VERTEX_POINT('',#32504);
#9297=VERTEX_POINT('',#32508);
#9298=VERTEX_POINT('',#32509);
#9299=VERTEX_POINT('',#32511);
#9300=VERTEX_POINT('',#32513);
#9301=VERTEX_POINT('',#32517);
#9302=VERTEX_POINT('',#32518);
#9303=VERTEX_POINT('',#32520);
#9304=VERTEX_POINT('',#32522);
#9305=VERTEX_POINT('',#32526);
#9306=VERTEX_POINT('',#32527);
#9307=VERTEX_POINT('',#32529);
#9308=VERTEX_POINT('',#32531);
#9309=VERTEX_POINT('',#32535);
#9310=VERTEX_POINT('',#32536);
#9311=VERTEX_POINT('',#32538);
#9312=VERTEX_POINT('',#32540);
#9313=VERTEX_POINT('',#32544);
#9314=VERTEX_POINT('',#32545);
#9315=VERTEX_POINT('',#32547);
#9316=VERTEX_POINT('',#32549);
#9317=VERTEX_POINT('',#32553);
#9318=VERTEX_POINT('',#32554);
#9319=VERTEX_POINT('',#32556);
#9320=VERTEX_POINT('',#32558);
#9321=VERTEX_POINT('',#32562);
#9322=VERTEX_POINT('',#32563);
#9323=VERTEX_POINT('',#32565);
#9324=VERTEX_POINT('',#32567);
#9325=VERTEX_POINT('',#32571);
#9326=VERTEX_POINT('',#32572);
#9327=VERTEX_POINT('',#32574);
#9328=VERTEX_POINT('',#32576);
#9329=VERTEX_POINT('',#32580);
#9330=VERTEX_POINT('',#32581);
#9331=VERTEX_POINT('',#32583);
#9332=VERTEX_POINT('',#32585);
#9333=VERTEX_POINT('',#32589);
#9334=VERTEX_POINT('',#32590);
#9335=VERTEX_POINT('',#32592);
#9336=VERTEX_POINT('',#32594);
#9337=VERTEX_POINT('',#32598);
#9338=VERTEX_POINT('',#32599);
#9339=VERTEX_POINT('',#32601);
#9340=VERTEX_POINT('',#32603);
#9341=VERTEX_POINT('',#32607);
#9342=VERTEX_POINT('',#32608);
#9343=VERTEX_POINT('',#32610);
#9344=VERTEX_POINT('',#32612);
#9345=VERTEX_POINT('',#32616);
#9346=VERTEX_POINT('',#32617);
#9347=VERTEX_POINT('',#32619);
#9348=VERTEX_POINT('',#32621);
#9349=VERTEX_POINT('',#32625);
#9350=VERTEX_POINT('',#32626);
#9351=VERTEX_POINT('',#32628);
#9352=VERTEX_POINT('',#32630);
#9353=VERTEX_POINT('',#32634);
#9354=VERTEX_POINT('',#32635);
#9355=VERTEX_POINT('',#32637);
#9356=VERTEX_POINT('',#32639);
#9357=VERTEX_POINT('',#32643);
#9358=VERTEX_POINT('',#32644);
#9359=VERTEX_POINT('',#32646);
#9360=VERTEX_POINT('',#32648);
#9361=VERTEX_POINT('',#32652);
#9362=VERTEX_POINT('',#32653);
#9363=VERTEX_POINT('',#32655);
#9364=VERTEX_POINT('',#32657);
#9365=VERTEX_POINT('',#32661);
#9366=VERTEX_POINT('',#32662);
#9367=VERTEX_POINT('',#32664);
#9368=VERTEX_POINT('',#32666);
#9369=VERTEX_POINT('',#32670);
#9370=VERTEX_POINT('',#32671);
#9371=VERTEX_POINT('',#32673);
#9372=VERTEX_POINT('',#32675);
#9373=VERTEX_POINT('',#32679);
#9374=VERTEX_POINT('',#32680);
#9375=VERTEX_POINT('',#32682);
#9376=VERTEX_POINT('',#32684);
#9377=VERTEX_POINT('',#32688);
#9378=VERTEX_POINT('',#32689);
#9379=VERTEX_POINT('',#32691);
#9380=VERTEX_POINT('',#32693);
#9381=VERTEX_POINT('',#32697);
#9382=VERTEX_POINT('',#32698);
#9383=VERTEX_POINT('',#32700);
#9384=VERTEX_POINT('',#32702);
#9385=VERTEX_POINT('',#32706);
#9386=VERTEX_POINT('',#32707);
#9387=VERTEX_POINT('',#32709);
#9388=VERTEX_POINT('',#32711);
#9389=VERTEX_POINT('',#32715);
#9390=VERTEX_POINT('',#32716);
#9391=VERTEX_POINT('',#32718);
#9392=VERTEX_POINT('',#32720);
#9393=VERTEX_POINT('',#32724);
#9394=VERTEX_POINT('',#32725);
#9395=VERTEX_POINT('',#32727);
#9396=VERTEX_POINT('',#32729);
#9397=VERTEX_POINT('',#32733);
#9398=VERTEX_POINT('',#32734);
#9399=VERTEX_POINT('',#32736);
#9400=VERTEX_POINT('',#32738);
#9401=VERTEX_POINT('',#32742);
#9402=VERTEX_POINT('',#32743);
#9403=VERTEX_POINT('',#32745);
#9404=VERTEX_POINT('',#32747);
#9405=VERTEX_POINT('',#32751);
#9406=VERTEX_POINT('',#32752);
#9407=VERTEX_POINT('',#32754);
#9408=VERTEX_POINT('',#32756);
#9409=VERTEX_POINT('',#32760);
#9410=VERTEX_POINT('',#32761);
#9411=VERTEX_POINT('',#32763);
#9412=VERTEX_POINT('',#32765);
#9413=VERTEX_POINT('',#32769);
#9414=VERTEX_POINT('',#32770);
#9415=VERTEX_POINT('',#32772);
#9416=VERTEX_POINT('',#32774);
#9417=VERTEX_POINT('',#32778);
#9418=VERTEX_POINT('',#32780);
#9419=VERTEX_POINT('',#32826);
#9420=VERTEX_POINT('',#32829);
#9421=VERTEX_POINT('',#32833);
#9422=VERTEX_POINT('',#32924);
#9423=VERTEX_POINT('',#32931);
#9424=VERTEX_POINT('',#32932);
#9425=VERTEX_POINT('',#32934);
#9426=VERTEX_POINT('',#32939);
#9427=VERTEX_POINT('',#32940);
#9428=VERTEX_POINT('',#32945);
#9429=VERTEX_POINT('',#32948);
#9430=VERTEX_POINT('',#32952);
#9431=VERTEX_POINT('',#32958);
#9432=VERTEX_POINT('',#32959);
#9433=VERTEX_POINT('',#32961);
#9434=VERTEX_POINT('',#32963);
#9435=VERTEX_POINT('',#32967);
#9436=VERTEX_POINT('',#32969);
#9437=VERTEX_POINT('',#32973);
#9438=VERTEX_POINT('',#32975);
#9439=VERTEX_POINT('',#32979);
#9440=VERTEX_POINT('',#32981);
#9441=VERTEX_POINT('',#32985);
#9442=VERTEX_POINT('',#32986);
#9443=VERTEX_POINT('',#32988);
#9444=VERTEX_POINT('',#32990);
#9445=VERTEX_POINT('',#32994);
#9446=VERTEX_POINT('',#32996);
#9447=VERTEX_POINT('',#33000);
#9448=VERTEX_POINT('',#33002);
#9449=VERTEX_POINT('',#33006);
#9450=VERTEX_POINT('',#33008);
#9451=VERTEX_POINT('',#33012);
#9452=VERTEX_POINT('',#33013);
#9453=VERTEX_POINT('',#33015);
#9454=VERTEX_POINT('',#33017);
#9455=VERTEX_POINT('',#33021);
#9456=VERTEX_POINT('',#33023);
#9457=VERTEX_POINT('',#33027);
#9458=VERTEX_POINT('',#33029);
#9459=VERTEX_POINT('',#33033);
#9460=VERTEX_POINT('',#33035);
#9461=VERTEX_POINT('',#33039);
#9462=VERTEX_POINT('',#33040);
#9463=VERTEX_POINT('',#33042);
#9464=VERTEX_POINT('',#33044);
#9465=VERTEX_POINT('',#33048);
#9466=VERTEX_POINT('',#33050);
#9467=VERTEX_POINT('',#33054);
#9468=VERTEX_POINT('',#33056);
#9469=VERTEX_POINT('',#33060);
#9470=VERTEX_POINT('',#33062);
#9471=VERTEX_POINT('',#33066);
#9472=VERTEX_POINT('',#33067);
#9473=VERTEX_POINT('',#33069);
#9474=VERTEX_POINT('',#33071);
#9475=VERTEX_POINT('',#33075);
#9476=VERTEX_POINT('',#33077);
#9477=VERTEX_POINT('',#33081);
#9478=VERTEX_POINT('',#33083);
#9479=VERTEX_POINT('',#33087);
#9480=VERTEX_POINT('',#33089);
#9481=VERTEX_POINT('',#33093);
#9482=VERTEX_POINT('',#33095);
#9483=VERTEX_POINT('',#33099);
#9484=VERTEX_POINT('',#33101);
#9485=VERTEX_POINT('',#33105);
#9486=VERTEX_POINT('',#33107);
#9487=VERTEX_POINT('',#33111);
#9488=VERTEX_POINT('',#33113);
#9489=VERTEX_POINT('',#33117);
#9490=VERTEX_POINT('',#33119);
#9491=VERTEX_POINT('',#33126);
#9492=VERTEX_POINT('',#33128);
#9493=VERTEX_POINT('',#33130);
#9494=VERTEX_POINT('',#33134);
#9495=VERTEX_POINT('',#33139);
#9496=VERTEX_POINT('',#33143);
#9497=VERTEX_POINT('',#33151);
#9498=VERTEX_POINT('',#33155);
#9499=VERTEX_POINT('',#33165);
#9500=VERTEX_POINT('',#33166);
#9501=VERTEX_POINT('',#33168);
#9502=VERTEX_POINT('',#33170);
#9503=VERTEX_POINT('',#33174);
#9504=VERTEX_POINT('',#33175);
#9505=VERTEX_POINT('',#33177);
#9506=VERTEX_POINT('',#33179);
#9507=VERTEX_POINT('',#33186);
#9508=VERTEX_POINT('',#33188);
#9509=VERTEX_POINT('',#33190);
#9510=VERTEX_POINT('',#33194);
#9511=VERTEX_POINT('',#33198);
#9512=VERTEX_POINT('',#33200);
#9513=VERTEX_POINT('',#33210);
#9514=VERTEX_POINT('',#33211);
#9515=VERTEX_POINT('',#33213);
#9516=VERTEX_POINT('',#33215);
#9517=VERTEX_POINT('',#33219);
#9518=VERTEX_POINT('',#33220);
#9519=VERTEX_POINT('',#33225);
#9520=VERTEX_POINT('',#33226);
#9521=VERTEX_POINT('',#33231);
#9522=VERTEX_POINT('',#33232);
#9523=VERTEX_POINT('',#33237);
#9524=VERTEX_POINT('',#33238);
#9525=VERTEX_POINT('',#33243);
#9526=VERTEX_POINT('',#33244);
#9527=VERTEX_POINT('',#33249);
#9528=VERTEX_POINT('',#33250);
#9529=VERTEX_POINT('',#33255);
#9530=VERTEX_POINT('',#33256);
#9531=VERTEX_POINT('',#33261);
#9532=VERTEX_POINT('',#33262);
#9533=VERTEX_POINT('',#33264);
#9534=VERTEX_POINT('',#33266);
#9535=VERTEX_POINT('',#33270);
#9536=VERTEX_POINT('',#33272);
#9537=VERTEX_POINT('',#33276);
#9538=VERTEX_POINT('',#33278);
#9539=VERTEX_POINT('',#33282);
#9540=VERTEX_POINT('',#33284);
#9541=VERTEX_POINT('',#33288);
#9542=VERTEX_POINT('',#33290);
#9543=VERTEX_POINT('',#33294);
#9544=VERTEX_POINT('',#33296);
#9545=VERTEX_POINT('',#33304);
#9546=VERTEX_POINT('',#33306);
#9547=VERTEX_POINT('',#33308);
#9548=VERTEX_POINT('',#33310);
#9549=VERTEX_POINT('',#33312);
#9550=VERTEX_POINT('',#33313);
#9551=VERTEX_POINT('',#33315);
#9552=VERTEX_POINT('',#33317);
#9553=VERTEX_POINT('',#33319);
#9554=VERTEX_POINT('',#33321);
#9555=VERTEX_POINT('',#33323);
#9556=VERTEX_POINT('',#33325);
#9557=VERTEX_POINT('',#33331);
#9558=VERTEX_POINT('',#33335);
#9559=VERTEX_POINT('',#33339);
#9560=VERTEX_POINT('',#33343);
#9561=VERTEX_POINT('',#33347);
#9562=VERTEX_POINT('',#33349);
#9563=VERTEX_POINT('',#33353);
#9564=VERTEX_POINT('',#33357);
#9565=VERTEX_POINT('',#33361);
#9566=VERTEX_POINT('',#33365);
#9567=VERTEX_POINT('',#33369);
#9568=VERTEX_POINT('',#33373);
#9569=VERTEX_POINT('',#33381);
#9570=VERTEX_POINT('',#33382);
#9571=VERTEX_POINT('',#33384);
#9572=VERTEX_POINT('',#33386);
#9573=VERTEX_POINT('',#33390);
#9574=VERTEX_POINT('',#33392);
#9575=VERTEX_POINT('',#33396);
#9576=VERTEX_POINT('',#33398);
#9577=VERTEX_POINT('',#33402);
#9578=VERTEX_POINT('',#33404);
#9579=VERTEX_POINT('',#33408);
#9580=VERTEX_POINT('',#33409);
#9581=VERTEX_POINT('',#33411);
#9582=VERTEX_POINT('',#33413);
#9583=VERTEX_POINT('',#33417);
#9584=VERTEX_POINT('',#33419);
#9585=VERTEX_POINT('',#33423);
#9586=VERTEX_POINT('',#33425);
#9587=VERTEX_POINT('',#33429);
#9588=VERTEX_POINT('',#33431);
#9589=VERTEX_POINT('',#33435);
#9590=VERTEX_POINT('',#33436);
#9591=VERTEX_POINT('',#33438);
#9592=VERTEX_POINT('',#33440);
#9593=VERTEX_POINT('',#33444);
#9594=VERTEX_POINT('',#33446);
#9595=VERTEX_POINT('',#33450);
#9596=VERTEX_POINT('',#33452);
#9597=VERTEX_POINT('',#33456);
#9598=VERTEX_POINT('',#33458);
#9599=VERTEX_POINT('',#33462);
#9600=VERTEX_POINT('',#33463);
#9601=VERTEX_POINT('',#33465);
#9602=VERTEX_POINT('',#33467);
#9603=VERTEX_POINT('',#33471);
#9604=VERTEX_POINT('',#33473);
#9605=VERTEX_POINT('',#33477);
#9606=VERTEX_POINT('',#33479);
#9607=VERTEX_POINT('',#33483);
#9608=VERTEX_POINT('',#33485);
#9609=VERTEX_POINT('',#33489);
#9610=VERTEX_POINT('',#33490);
#9611=VERTEX_POINT('',#33492);
#9612=VERTEX_POINT('',#33494);
#9613=VERTEX_POINT('',#33498);
#9614=VERTEX_POINT('',#33500);
#9615=VERTEX_POINT('',#33504);
#9616=VERTEX_POINT('',#33506);
#9617=VERTEX_POINT('',#33510);
#9618=VERTEX_POINT('',#33512);
#9619=VERTEX_POINT('',#33516);
#9620=VERTEX_POINT('',#33518);
#9621=VERTEX_POINT('',#33522);
#9622=VERTEX_POINT('',#33524);
#9623=VERTEX_POINT('',#33528);
#9624=VERTEX_POINT('',#33530);
#9625=VERTEX_POINT('',#33534);
#9626=VERTEX_POINT('',#33536);
#9627=VERTEX_POINT('',#33540);
#9628=VERTEX_POINT('',#33542);
#9629=VERTEX_POINT('',#33549);
#9630=VERTEX_POINT('',#33551);
#9631=VERTEX_POINT('',#33553);
#9632=VERTEX_POINT('',#33557);
#9633=VERTEX_POINT('',#33562);
#9634=VERTEX_POINT('',#33566);
#9635=VERTEX_POINT('',#33574);
#9636=VERTEX_POINT('',#33576);
#9637=VERTEX_POINT('',#33588);
#9638=VERTEX_POINT('',#33589);
#9639=VERTEX_POINT('',#33591);
#9640=VERTEX_POINT('',#33593);
#9641=VERTEX_POINT('',#33597);
#9642=VERTEX_POINT('',#33599);
#9643=VERTEX_POINT('',#33603);
#9644=VERTEX_POINT('',#33605);
#9645=VERTEX_POINT('',#33612);
#9646=VERTEX_POINT('',#33613);
#9647=VERTEX_POINT('',#33615);
#9648=VERTEX_POINT('',#33617);
#9649=VERTEX_POINT('',#33621);
#9650=VERTEX_POINT('',#33623);
#9651=VERTEX_POINT('',#33627);
#9652=VERTEX_POINT('',#33629);
#9653=VERTEX_POINT('',#33636);
#9654=VERTEX_POINT('',#33637);
#9655=VERTEX_POINT('',#33639);
#9656=VERTEX_POINT('',#33641);
#9657=VERTEX_POINT('',#33645);
#9658=VERTEX_POINT('',#33647);
#9659=VERTEX_POINT('',#33651);
#9660=VERTEX_POINT('',#33653);
#9661=VERTEX_POINT('',#33660);
#9662=VERTEX_POINT('',#33661);
#9663=VERTEX_POINT('',#33663);
#9664=VERTEX_POINT('',#33665);
#9665=VERTEX_POINT('',#33669);
#9666=VERTEX_POINT('',#33671);
#9667=VERTEX_POINT('',#33675);
#9668=VERTEX_POINT('',#33677);
#9669=VERTEX_POINT('',#33684);
#9670=VERTEX_POINT('',#33685);
#9671=VERTEX_POINT('',#33687);
#9672=VERTEX_POINT('',#33689);
#9673=VERTEX_POINT('',#33693);
#9674=VERTEX_POINT('',#33695);
#9675=VERTEX_POINT('',#33699);
#9676=VERTEX_POINT('',#33701);
#9677=VERTEX_POINT('',#33708);
#9678=VERTEX_POINT('',#33709);
#9679=VERTEX_POINT('',#33711);
#9680=VERTEX_POINT('',#33713);
#9681=VERTEX_POINT('',#33717);
#9682=VERTEX_POINT('',#33719);
#9683=VERTEX_POINT('',#33723);
#9684=VERTEX_POINT('',#33725);
#9685=VERTEX_POINT('',#33732);
#9686=VERTEX_POINT('',#33733);
#9687=VERTEX_POINT('',#33735);
#9688=VERTEX_POINT('',#33737);
#9689=VERTEX_POINT('',#33741);
#9690=VERTEX_POINT('',#33743);
#9691=VERTEX_POINT('',#33747);
#9692=VERTEX_POINT('',#33749);
#9693=VERTEX_POINT('',#33753);
#9694=VERTEX_POINT('',#33755);
#9695=VERTEX_POINT('',#33757);
#9696=VERTEX_POINT('',#33759);
#9697=VERTEX_POINT('',#33763);
#9698=VERTEX_POINT('',#33765);
#9699=VERTEX_POINT('',#33767);
#9700=VERTEX_POINT('',#33771);
#9701=VERTEX_POINT('',#33773);
#9702=VERTEX_POINT('',#33777);
#9703=VERTEX_POINT('',#33779);
#9704=VERTEX_POINT('',#33781);
#9705=VERTEX_POINT('',#33783);
#9706=VERTEX_POINT('',#33785);
#9707=VERTEX_POINT('',#33787);
#9708=VERTEX_POINT('',#33789);
#9709=VERTEX_POINT('',#33791);
#9710=VERTEX_POINT('',#33793);
#9711=VERTEX_POINT('',#33797);
#9712=VERTEX_POINT('',#33798);
#9713=VERTEX_POINT('',#33803);
#9714=VERTEX_POINT('',#33804);
#9715=VERTEX_POINT('',#33806);
#9716=VERTEX_POINT('',#33808);
#9717=VERTEX_POINT('',#33815);
#9718=VERTEX_POINT('',#33817);
#9719=VERTEX_POINT('',#33819);
#9720=VERTEX_POINT('',#33824);
#9721=VERTEX_POINT('',#33826);
#9722=VERTEX_POINT('',#33829);
#9723=VERTEX_POINT('',#33831);
#9724=VERTEX_POINT('',#33833);
#9725=VERTEX_POINT('',#33835);
#9726=VERTEX_POINT('',#33839);
#9727=VERTEX_POINT('',#33840);
#9728=VERTEX_POINT('',#33845);
#9729=VERTEX_POINT('',#33847);
#9730=VERTEX_POINT('',#33853);
#9731=VERTEX_POINT('',#33854);
#9732=VERTEX_POINT('',#33856);
#9733=VERTEX_POINT('',#33858);
#9734=VERTEX_POINT('',#33862);
#9735=VERTEX_POINT('',#33864);
#9736=VERTEX_POINT('',#33868);
#9737=VERTEX_POINT('',#33870);
#9738=VERTEX_POINT('',#33875);
#9739=VERTEX_POINT('',#33877);
#9740=VERTEX_POINT('',#33888);
#9741=VERTEX_POINT('',#33890);
#9742=VERTEX_POINT('',#33892);
#9743=VERTEX_POINT('',#33896);
#9744=VERTEX_POINT('',#33900);
#9745=VERTEX_POINT('',#33902);
#9746=VERTEX_POINT('',#33907);
#9747=VERTEX_POINT('',#33919);
#9748=VERTEX_POINT('',#33921);
#9749=VERTEX_POINT('',#33925);
#9750=VERTEX_POINT('',#33927);
#9751=VERTEX_POINT('',#33934);
#9752=VERTEX_POINT('',#33935);
#9753=VERTEX_POINT('',#33937);
#9754=VERTEX_POINT('',#33939);
#9755=VERTEX_POINT('',#33943);
#9756=VERTEX_POINT('',#33945);
#9757=VERTEX_POINT('',#33949);
#9758=VERTEX_POINT('',#33951);
#9759=VERTEX_POINT('',#33955);
#9760=VERTEX_POINT('',#33957);
#9761=VERTEX_POINT('',#33961);
#9762=VERTEX_POINT('',#33962);
#9763=VERTEX_POINT('',#33964);
#9764=VERTEX_POINT('',#33966);
#9765=VERTEX_POINT('',#33970);
#9766=VERTEX_POINT('',#33972);
#9767=VERTEX_POINT('',#33976);
#9768=VERTEX_POINT('',#33978);
#9769=VERTEX_POINT('',#33982);
#9770=VERTEX_POINT('',#33984);
#9771=VERTEX_POINT('',#33988);
#9772=VERTEX_POINT('',#33989);
#9773=VERTEX_POINT('',#33991);
#9774=VERTEX_POINT('',#33993);
#9775=VERTEX_POINT('',#33997);
#9776=VERTEX_POINT('',#33999);
#9777=VERTEX_POINT('',#34003);
#9778=VERTEX_POINT('',#34005);
#9779=VERTEX_POINT('',#34009);
#9780=VERTEX_POINT('',#34011);
#9781=VERTEX_POINT('',#34015);
#9782=VERTEX_POINT('',#34016);
#9783=VERTEX_POINT('',#34018);
#9784=VERTEX_POINT('',#34020);
#9785=VERTEX_POINT('',#34024);
#9786=VERTEX_POINT('',#34026);
#9787=VERTEX_POINT('',#34030);
#9788=VERTEX_POINT('',#34032);
#9789=VERTEX_POINT('',#34036);
#9790=VERTEX_POINT('',#34038);
#9791=VERTEX_POINT('',#34042);
#9792=VERTEX_POINT('',#34043);
#9793=VERTEX_POINT('',#34045);
#9794=VERTEX_POINT('',#34047);
#9795=VERTEX_POINT('',#34051);
#9796=VERTEX_POINT('',#34053);
#9797=VERTEX_POINT('',#34057);
#9798=VERTEX_POINT('',#34059);
#9799=VERTEX_POINT('',#34063);
#9800=VERTEX_POINT('',#34065);
#9801=VERTEX_POINT('',#34069);
#9802=VERTEX_POINT('',#34071);
#9803=VERTEX_POINT('',#34075);
#9804=VERTEX_POINT('',#34077);
#9805=VERTEX_POINT('',#34081);
#9806=VERTEX_POINT('',#34083);
#9807=VERTEX_POINT('',#34087);
#9808=VERTEX_POINT('',#34089);
#9809=VERTEX_POINT('',#34093);
#9810=VERTEX_POINT('',#34095);
#9811=VERTEX_POINT('',#34102);
#9812=VERTEX_POINT('',#34104);
#9813=VERTEX_POINT('',#34106);
#9814=VERTEX_POINT('',#34110);
#9815=VERTEX_POINT('',#34115);
#9816=VERTEX_POINT('',#34119);
#9817=VERTEX_POINT('',#34127);
#9818=VERTEX_POINT('',#34131);
#9819=VERTEX_POINT('',#34141);
#9820=VERTEX_POINT('',#34142);
#9821=VERTEX_POINT('',#34144);
#9822=VERTEX_POINT('',#34146);
#9823=VERTEX_POINT('',#34150);
#9824=VERTEX_POINT('',#34152);
#9825=VERTEX_POINT('',#34156);
#9826=VERTEX_POINT('',#34158);
#9827=VERTEX_POINT('',#34162);
#9828=VERTEX_POINT('',#34164);
#9829=VERTEX_POINT('',#34168);
#9830=VERTEX_POINT('',#34169);
#9831=VERTEX_POINT('',#34171);
#9832=VERTEX_POINT('',#34173);
#9833=VERTEX_POINT('',#34177);
#9834=VERTEX_POINT('',#34179);
#9835=VERTEX_POINT('',#34183);
#9836=VERTEX_POINT('',#34185);
#9837=VERTEX_POINT('',#34189);
#9838=VERTEX_POINT('',#34191);
#9839=VERTEX_POINT('',#34195);
#9840=VERTEX_POINT('',#34196);
#9841=VERTEX_POINT('',#34198);
#9842=VERTEX_POINT('',#34200);
#9843=VERTEX_POINT('',#34204);
#9844=VERTEX_POINT('',#34206);
#9845=VERTEX_POINT('',#34210);
#9846=VERTEX_POINT('',#34212);
#9847=VERTEX_POINT('',#34216);
#9848=VERTEX_POINT('',#34218);
#9849=VERTEX_POINT('',#34222);
#9850=VERTEX_POINT('',#34223);
#9851=VERTEX_POINT('',#34225);
#9852=VERTEX_POINT('',#34227);
#9853=VERTEX_POINT('',#34231);
#9854=VERTEX_POINT('',#34233);
#9855=VERTEX_POINT('',#34237);
#9856=VERTEX_POINT('',#34239);
#9857=VERTEX_POINT('',#34243);
#9858=VERTEX_POINT('',#34245);
#9859=VERTEX_POINT('',#34249);
#9860=VERTEX_POINT('',#34250);
#9861=VERTEX_POINT('',#34252);
#9862=VERTEX_POINT('',#34254);
#9863=VERTEX_POINT('',#34258);
#9864=VERTEX_POINT('',#34260);
#9865=VERTEX_POINT('',#34264);
#9866=VERTEX_POINT('',#34266);
#9867=VERTEX_POINT('',#34270);
#9868=VERTEX_POINT('',#34272);
#9869=VERTEX_POINT('',#34276);
#9870=VERTEX_POINT('',#34278);
#9871=VERTEX_POINT('',#34282);
#9872=VERTEX_POINT('',#34284);
#9873=VERTEX_POINT('',#34288);
#9874=VERTEX_POINT('',#34290);
#9875=VERTEX_POINT('',#34294);
#9876=VERTEX_POINT('',#34296);
#9877=VERTEX_POINT('',#34300);
#9878=VERTEX_POINT('',#34302);
#9879=VERTEX_POINT('',#34309);
#9880=VERTEX_POINT('',#34311);
#9881=VERTEX_POINT('',#34313);
#9882=VERTEX_POINT('',#34317);
#9883=VERTEX_POINT('',#34322);
#9884=VERTEX_POINT('',#34326);
#9885=VERTEX_POINT('',#34334);
#9886=VERTEX_POINT('',#34338);
#9887=VERTEX_POINT('',#34348);
#9888=VERTEX_POINT('',#34349);
#9889=VERTEX_POINT('',#34351);
#9890=VERTEX_POINT('',#34356);
#9891=VERTEX_POINT('',#34357);
#9892=VERTEX_POINT('',#34362);
#9893=VERTEX_POINT('',#34365);
#9894=VERTEX_POINT('',#34369);
#9895=VERTEX_POINT('',#34375);
#9896=VERTEX_POINT('',#34376);
#9897=VERTEX_POINT('',#34378);
#9898=VERTEX_POINT('',#34380);
#9899=VERTEX_POINT('',#34384);
#9900=VERTEX_POINT('',#34385);
#9901=VERTEX_POINT('',#34387);
#9902=VERTEX_POINT('',#34389);
#9903=VERTEX_POINT('',#34393);
#9904=VERTEX_POINT('',#34394);
#9905=VERTEX_POINT('',#34402);
#9906=VERTEX_POINT('',#34404);
#9907=VERTEX_POINT('',#34408);
#9908=VERTEX_POINT('',#34412);
#9909=VERTEX_POINT('',#34420);
#9910=VERTEX_POINT('',#34421);
#9911=VERTEX_POINT('',#34423);
#9912=VERTEX_POINT('',#34428);
#9913=VERTEX_POINT('',#34433);
#9914=VERTEX_POINT('',#34434);
#9915=VERTEX_POINT('',#34445);
#9916=VERTEX_POINT('',#34447);
#9917=VERTEX_POINT('',#34460);
#9918=VERTEX_POINT('',#34464);
#9919=VERTEX_POINT('',#34470);
#9920=VERTEX_POINT('',#34471);
#9921=VERTEX_POINT('',#34482);
#9922=VERTEX_POINT('',#34484);
#9923=VERTEX_POINT('',#34497);
#9924=VERTEX_POINT('',#34501);
#9925=VERTEX_POINT('',#34507);
#9926=VERTEX_POINT('',#34508);
#9927=VERTEX_POINT('',#34519);
#9928=VERTEX_POINT('',#34521);
#9929=VERTEX_POINT('',#34534);
#9930=VERTEX_POINT('',#34538);
#9931=VERTEX_POINT('',#34540);
#9932=VERTEX_POINT('',#34546);
#9933=VERTEX_POINT('',#34547);
#9934=VERTEX_POINT('',#34558);
#9935=VERTEX_POINT('',#34560);
#9936=VERTEX_POINT('',#34573);
#9937=VERTEX_POINT('',#34577);
#9938=VERTEX_POINT('',#34583);
#9939=VERTEX_POINT('',#34584);
#9940=VERTEX_POINT('',#34586);
#9941=VERTEX_POINT('',#34591);
#9942=VERTEX_POINT('',#34593);
#9943=VERTEX_POINT('',#34605);
#9944=VERTEX_POINT('',#34607);
#9945=VERTEX_POINT('',#34619);
#9946=VERTEX_POINT('',#34621);
#9947=VERTEX_POINT('',#34633);
#9948=VERTEX_POINT('',#34635);
#9949=VERTEX_POINT('',#34648);
#9950=VERTEX_POINT('',#34652);
#9951=VERTEX_POINT('',#34654);
#9952=VERTEX_POINT('',#34675);
#9953=VERTEX_POINT('',#34681);
#9954=VERTEX_POINT('',#34698);
#9955=VERTEX_POINT('',#34712);
#9956=VERTEX_POINT('',#34718);
#9957=VERTEX_POINT('',#34739);
#9958=VERTEX_POINT('',#34760);
#9959=VERTEX_POINT('',#34763);
#9960=VERTEX_POINT('',#34765);
#9961=EDGE_CURVE('',#8073,#8073,#6993,.T.);
#9962=EDGE_CURVE('',#8073,#8074,#6994,.T.);
#9963=EDGE_CURVE('',#8074,#8075,#6995,.T.);
#9964=EDGE_CURVE('',#8075,#8074,#6996,.T.);
#9965=EDGE_CURVE('',#8075,#8076,#1083,.T.);
#9966=EDGE_CURVE('',#8077,#8076,#6997,.T.);
#9967=EDGE_CURVE('',#8076,#8077,#6998,.T.);
#9968=EDGE_CURVE('',#8078,#8078,#6999,.T.);
#9969=EDGE_CURVE('',#8077,#8079,#7000,.T.);
#9970=EDGE_CURVE('',#8079,#8079,#7001,.T.);
#9971=EDGE_CURVE('',#8080,#8080,#7002,.T.);
#9972=EDGE_CURVE('',#8080,#8078,#1084,.T.);
#9973=EDGE_CURVE('',#8081,#8082,#7003,.T.);
#9974=EDGE_CURVE('',#8082,#8083,#1085,.T.);
#9975=EDGE_CURVE('',#8083,#8084,#7004,.T.);
#9976=EDGE_CURVE('',#8084,#8081,#1086,.T.);
#9977=EDGE_CURVE('',#8085,#8082,#7005,.T.);
#9978=EDGE_CURVE('',#8086,#8085,#1087,.T.);
#9979=EDGE_CURVE('',#8083,#8086,#7006,.T.);
#9980=EDGE_CURVE('',#8085,#8087,#7007,.T.);
#9981=EDGE_CURVE('',#8087,#8088,#1088,.T.);
#9982=EDGE_CURVE('',#8088,#8086,#7008,.T.);
#9983=EDGE_CURVE('',#8089,#8087,#1089,.T.);
#9984=EDGE_CURVE('',#8090,#8089,#1090,.T.);
#9985=EDGE_CURVE('',#8088,#8090,#1091,.T.);
#9986=EDGE_CURVE('',#8091,#8092,#7009,.T.);
#9987=EDGE_CURVE('',#8092,#8093,#1092,.T.);
#9988=EDGE_CURVE('',#8093,#8094,#7010,.T.);
#9989=EDGE_CURVE('',#8094,#8091,#1093,.T.);
#9990=EDGE_CURVE('',#8095,#8092,#7011,.T.);
#9991=EDGE_CURVE('',#8096,#8095,#1094,.T.);
#9992=EDGE_CURVE('',#8093,#8096,#7012,.T.);
#9993=EDGE_CURVE('',#8095,#8097,#7013,.T.);
#9994=EDGE_CURVE('',#8097,#8098,#1095,.T.);
#9995=EDGE_CURVE('',#8098,#8096,#7014,.T.);
#9996=EDGE_CURVE('',#8099,#8097,#1096,.T.);
#9997=EDGE_CURVE('',#8100,#8099,#1097,.T.);
#9998=EDGE_CURVE('',#8098,#8100,#1098,.T.);
#9999=EDGE_CURVE('',#8101,#8102,#7015,.T.);
#10000=EDGE_CURVE('',#8102,#8103,#1099,.T.);
#10001=EDGE_CURVE('',#8103,#8104,#7016,.T.);
#10002=EDGE_CURVE('',#8104,#8101,#1100,.T.);
#10003=EDGE_CURVE('',#8105,#8102,#7017,.T.);
#10004=EDGE_CURVE('',#8106,#8105,#1101,.T.);
#10005=EDGE_CURVE('',#8103,#8106,#7018,.T.);
#10006=EDGE_CURVE('',#8105,#8107,#7019,.T.);
#10007=EDGE_CURVE('',#8107,#8108,#1102,.T.);
#10008=EDGE_CURVE('',#8108,#8106,#7020,.T.);
#10009=EDGE_CURVE('',#8109,#8107,#1103,.T.);
#10010=EDGE_CURVE('',#8110,#8109,#1104,.T.);
#10011=EDGE_CURVE('',#8108,#8110,#1105,.T.);
#10012=EDGE_CURVE('',#8111,#8112,#7021,.T.);
#10013=EDGE_CURVE('',#8112,#8113,#1106,.T.);
#10014=EDGE_CURVE('',#8113,#8114,#7022,.T.);
#10015=EDGE_CURVE('',#8114,#8111,#1107,.T.);
#10016=EDGE_CURVE('',#8115,#8112,#7023,.T.);
#10017=EDGE_CURVE('',#8116,#8115,#1108,.T.);
#10018=EDGE_CURVE('',#8113,#8116,#7024,.T.);
#10019=EDGE_CURVE('',#8115,#8117,#7025,.T.);
#10020=EDGE_CURVE('',#8117,#8118,#1109,.T.);
#10021=EDGE_CURVE('',#8118,#8116,#7026,.T.);
#10022=EDGE_CURVE('',#8119,#8117,#1110,.T.);
#10023=EDGE_CURVE('',#8120,#8119,#1111,.T.);
#10024=EDGE_CURVE('',#8118,#8120,#1112,.T.);
#10025=EDGE_CURVE('',#8121,#8122,#7027,.T.);
#10026=EDGE_CURVE('',#8122,#8123,#1113,.T.);
#10027=EDGE_CURVE('',#8123,#8124,#7028,.T.);
#10028=EDGE_CURVE('',#8124,#8121,#1114,.T.);
#10029=EDGE_CURVE('',#8125,#8122,#7029,.T.);
#10030=EDGE_CURVE('',#8126,#8125,#1115,.T.);
#10031=EDGE_CURVE('',#8123,#8126,#7030,.T.);
#10032=EDGE_CURVE('',#8125,#8127,#7031,.T.);
#10033=EDGE_CURVE('',#8127,#8128,#1116,.T.);
#10034=EDGE_CURVE('',#8128,#8126,#7032,.T.);
#10035=EDGE_CURVE('',#8129,#8127,#1117,.T.);
#10036=EDGE_CURVE('',#8130,#8129,#1118,.T.);
#10037=EDGE_CURVE('',#8128,#8130,#1119,.T.);
#10038=EDGE_CURVE('',#8131,#8124,#1120,.T.);
#10039=EDGE_CURVE('',#8132,#8131,#1121,.T.);
#10040=EDGE_CURVE('',#8121,#8132,#1122,.T.);
#10041=EDGE_CURVE('',#8133,#8114,#1123,.T.);
#10042=EDGE_CURVE('',#8134,#8133,#1124,.T.);
#10043=EDGE_CURVE('',#8111,#8134,#1125,.T.);
#10044=EDGE_CURVE('',#8135,#8094,#1126,.T.);
#10045=EDGE_CURVE('',#8136,#8135,#1127,.T.);
#10046=EDGE_CURVE('',#8091,#8136,#1128,.T.);
#10047=EDGE_CURVE('',#8137,#8084,#1129,.T.);
#10048=EDGE_CURVE('',#8138,#8137,#1130,.T.);
#10049=EDGE_CURVE('',#8081,#8138,#1131,.T.);
#10050=EDGE_CURVE('',#8139,#8129,#7033,.T.);
#10051=EDGE_CURVE('',#8140,#8139,#1132,.T.);
#10052=EDGE_CURVE('',#8130,#8140,#7034,.T.);
#10053=EDGE_CURVE('',#8110,#8133,#7035,.T.);
#10054=EDGE_CURVE('',#8134,#8109,#7036,.T.);
#10055=EDGE_CURVE('',#8140,#8141,#1133,.T.);
#10056=EDGE_CURVE('',#8141,#8142,#7037,.T.);
#10057=EDGE_CURVE('',#8142,#8143,#1134,.T.);
#10058=EDGE_CURVE('',#8143,#8137,#7038,.T.);
#10059=EDGE_CURVE('',#8090,#8135,#7039,.T.);
#10060=EDGE_CURVE('',#8100,#8144,#7040,.T.);
#10061=EDGE_CURVE('',#8144,#8104,#1135,.T.);
#10062=EDGE_CURVE('',#8120,#8131,#7041,.T.);
#10063=EDGE_CURVE('',#8145,#8099,#7042,.T.);
#10064=EDGE_CURVE('',#8145,#8144,#1136,.T.);
#10065=EDGE_CURVE('',#8143,#8146,#1137,.T.);
#10066=EDGE_CURVE('',#8138,#8146,#7043,.T.);
#10067=EDGE_CURVE('',#8101,#8145,#1138,.T.);
#10068=EDGE_CURVE('',#8132,#8119,#7044,.T.);
#10069=EDGE_CURVE('',#8147,#8141,#1139,.T.);
#10070=EDGE_CURVE('',#8148,#8147,#7045,.T.);
#10071=EDGE_CURVE('',#8142,#8148,#1140,.T.);
#10072=EDGE_CURVE('',#8146,#8148,#1141,.T.);
#10073=EDGE_CURVE('',#8136,#8089,#7046,.T.);
#10074=EDGE_CURVE('',#8147,#8139,#1142,.T.);
#10075=EDGE_CURVE('',#8149,#8149,#7047,.T.);
#10076=EDGE_CURVE('',#8150,#8150,#7048,.T.);
#10077=EDGE_CURVE('',#8150,#8151,#1143,.T.);
#10078=EDGE_CURVE('',#8151,#8151,#7049,.T.);
#10079=EDGE_CURVE('',#8152,#8152,#7050,.T.);
#10080=EDGE_CURVE('',#8152,#8149,#1144,.T.);
#10081=EDGE_CURVE('',#8153,#8154,#236,.T.);
#10082=EDGE_CURVE('',#8153,#8155,#7051,.T.);
#10083=EDGE_CURVE('',#8156,#8155,#237,.T.);
#10084=EDGE_CURVE('',#8156,#8157,#1145,.T.);
#10085=EDGE_CURVE('',#8158,#8157,#238,.T.);
#10086=EDGE_CURVE('',#8159,#8158,#7052,.T.);
#10087=EDGE_CURVE('',#8160,#8159,#239,.T.);
#10088=EDGE_CURVE('',#8160,#8154,#1146,.T.);
#10089=EDGE_CURVE('',#8161,#8162,#1147,.T.);
#10090=EDGE_CURVE('',#8162,#8163,#200,.T.);
#10091=EDGE_CURVE('',#8163,#8164,#1148,.T.);
#10092=EDGE_CURVE('',#8164,#8161,#201,.T.);
#10093=EDGE_CURVE('',#8154,#8165,#1149,.T.);
#10094=EDGE_CURVE('',#8166,#8160,#1150,.T.);
#10095=EDGE_CURVE('',#8165,#8166,#1151,.T.);
#10096=EDGE_CURVE('',#8159,#8167,#1152,.T.);
#10097=EDGE_CURVE('',#8167,#8166,#240,.T.);
#10098=EDGE_CURVE('',#8168,#8158,#1153,.T.);
#10099=EDGE_CURVE('',#8168,#8167,#7053,.T.);
#10100=EDGE_CURVE('',#8169,#8168,#241,.T.);
#10101=EDGE_CURVE('',#8157,#8169,#1154,.T.);
#10102=EDGE_CURVE('',#8170,#8156,#1155,.T.);
#10103=EDGE_CURVE('',#8169,#8170,#1156,.T.);
#10104=EDGE_CURVE('',#8155,#8171,#1157,.T.);
#10105=EDGE_CURVE('',#8171,#8170,#242,.T.);
#10106=EDGE_CURVE('',#8165,#8172,#243,.T.);
#10107=EDGE_CURVE('',#8171,#8172,#7054,.T.);
#10108=EDGE_CURVE('',#8172,#8153,#1158,.T.);
#10109=EDGE_CURVE('',#8173,#8163,#1159,.T.);
#10110=EDGE_CURVE('',#8173,#8174,#1160,.T.);
#10111=EDGE_CURVE('',#8174,#8164,#1161,.T.);
#10112=EDGE_CURVE('',#8175,#8162,#1162,.T.);
#10113=EDGE_CURVE('',#8175,#8173,#7055,.T.);
#10114=EDGE_CURVE('',#8174,#8176,#7056,.T.);
#10115=EDGE_CURVE('',#8176,#8161,#1163,.T.);
#10116=EDGE_CURVE('',#8176,#8175,#1164,.T.);
#10117=EDGE_CURVE('',#8177,#8178,#244,.T.);
#10118=EDGE_CURVE('',#8177,#8179,#7057,.T.);
#10119=EDGE_CURVE('',#8180,#8179,#245,.T.);
#10120=EDGE_CURVE('',#8180,#8181,#1165,.T.);
#10121=EDGE_CURVE('',#8182,#8181,#246,.T.);
#10122=EDGE_CURVE('',#8183,#8182,#7058,.T.);
#10123=EDGE_CURVE('',#8184,#8183,#247,.T.);
#10124=EDGE_CURVE('',#8184,#8178,#1166,.T.);
#10125=EDGE_CURVE('',#8185,#8186,#1167,.T.);
#10126=EDGE_CURVE('',#8186,#8187,#202,.T.);
#10127=EDGE_CURVE('',#8187,#8188,#1168,.T.);
#10128=EDGE_CURVE('',#8188,#8185,#203,.T.);
#10129=EDGE_CURVE('',#8178,#8189,#1169,.T.);
#10130=EDGE_CURVE('',#8190,#8184,#1170,.T.);
#10131=EDGE_CURVE('',#8189,#8190,#1171,.T.);
#10132=EDGE_CURVE('',#8183,#8191,#1172,.T.);
#10133=EDGE_CURVE('',#8191,#8190,#248,.T.);
#10134=EDGE_CURVE('',#8192,#8182,#1173,.T.);
#10135=EDGE_CURVE('',#8192,#8191,#7059,.T.);
#10136=EDGE_CURVE('',#8193,#8192,#249,.T.);
#10137=EDGE_CURVE('',#8181,#8193,#1174,.T.);
#10138=EDGE_CURVE('',#8194,#8180,#1175,.T.);
#10139=EDGE_CURVE('',#8193,#8194,#1176,.T.);
#10140=EDGE_CURVE('',#8179,#8195,#1177,.T.);
#10141=EDGE_CURVE('',#8195,#8194,#250,.T.);
#10142=EDGE_CURVE('',#8189,#8196,#251,.T.);
#10143=EDGE_CURVE('',#8195,#8196,#7060,.T.);
#10144=EDGE_CURVE('',#8196,#8177,#1178,.T.);
#10145=EDGE_CURVE('',#8197,#8187,#1179,.T.);
#10146=EDGE_CURVE('',#8197,#8198,#1180,.T.);
#10147=EDGE_CURVE('',#8198,#8188,#1181,.T.);
#10148=EDGE_CURVE('',#8199,#8186,#1182,.T.);
#10149=EDGE_CURVE('',#8199,#8197,#7061,.T.);
#10150=EDGE_CURVE('',#8198,#8200,#7062,.T.);
#10151=EDGE_CURVE('',#8200,#8185,#1183,.T.);
#10152=EDGE_CURVE('',#8200,#8199,#1184,.T.);
#10153=EDGE_CURVE('',#8201,#8202,#252,.T.);
#10154=EDGE_CURVE('',#8201,#8203,#7063,.T.);
#10155=EDGE_CURVE('',#8204,#8203,#253,.T.);
#10156=EDGE_CURVE('',#8204,#8205,#1185,.T.);
#10157=EDGE_CURVE('',#8206,#8205,#254,.T.);
#10158=EDGE_CURVE('',#8207,#8206,#7064,.T.);
#10159=EDGE_CURVE('',#8208,#8207,#255,.T.);
#10160=EDGE_CURVE('',#8208,#8202,#1186,.T.);
#10161=EDGE_CURVE('',#8209,#8210,#1187,.T.);
#10162=EDGE_CURVE('',#8210,#8211,#204,.T.);
#10163=EDGE_CURVE('',#8211,#8212,#1188,.T.);
#10164=EDGE_CURVE('',#8212,#8209,#205,.T.);
#10165=EDGE_CURVE('',#8202,#8213,#1189,.T.);
#10166=EDGE_CURVE('',#8214,#8208,#1190,.T.);
#10167=EDGE_CURVE('',#8213,#8214,#1191,.T.);
#10168=EDGE_CURVE('',#8207,#8215,#1192,.T.);
#10169=EDGE_CURVE('',#8215,#8214,#256,.T.);
#10170=EDGE_CURVE('',#8216,#8206,#1193,.T.);
#10171=EDGE_CURVE('',#8216,#8215,#7065,.T.);
#10172=EDGE_CURVE('',#8217,#8216,#257,.T.);
#10173=EDGE_CURVE('',#8205,#8217,#1194,.T.);
#10174=EDGE_CURVE('',#8218,#8204,#1195,.T.);
#10175=EDGE_CURVE('',#8217,#8218,#1196,.T.);
#10176=EDGE_CURVE('',#8203,#8219,#1197,.T.);
#10177=EDGE_CURVE('',#8219,#8218,#258,.T.);
#10178=EDGE_CURVE('',#8213,#8220,#259,.T.);
#10179=EDGE_CURVE('',#8219,#8220,#7066,.T.);
#10180=EDGE_CURVE('',#8220,#8201,#1198,.T.);
#10181=EDGE_CURVE('',#8221,#8211,#1199,.T.);
#10182=EDGE_CURVE('',#8221,#8222,#1200,.T.);
#10183=EDGE_CURVE('',#8222,#8212,#1201,.T.);
#10184=EDGE_CURVE('',#8223,#8210,#1202,.T.);
#10185=EDGE_CURVE('',#8223,#8221,#7067,.T.);
#10186=EDGE_CURVE('',#8222,#8224,#7068,.T.);
#10187=EDGE_CURVE('',#8224,#8209,#1203,.T.);
#10188=EDGE_CURVE('',#8224,#8223,#1204,.T.);
#10189=EDGE_CURVE('',#8225,#8226,#260,.T.);
#10190=EDGE_CURVE('',#8225,#8227,#7069,.T.);
#10191=EDGE_CURVE('',#8228,#8227,#261,.T.);
#10192=EDGE_CURVE('',#8228,#8229,#1205,.T.);
#10193=EDGE_CURVE('',#8230,#8229,#262,.T.);
#10194=EDGE_CURVE('',#8231,#8230,#7070,.T.);
#10195=EDGE_CURVE('',#8232,#8231,#263,.T.);
#10196=EDGE_CURVE('',#8232,#8226,#1206,.T.);
#10197=EDGE_CURVE('',#8233,#8234,#1207,.T.);
#10198=EDGE_CURVE('',#8234,#8235,#206,.T.);
#10199=EDGE_CURVE('',#8235,#8236,#1208,.T.);
#10200=EDGE_CURVE('',#8236,#8233,#207,.T.);
#10201=EDGE_CURVE('',#8226,#8237,#1209,.T.);
#10202=EDGE_CURVE('',#8238,#8232,#1210,.T.);
#10203=EDGE_CURVE('',#8237,#8238,#1211,.T.);
#10204=EDGE_CURVE('',#8231,#8239,#1212,.T.);
#10205=EDGE_CURVE('',#8239,#8238,#264,.T.);
#10206=EDGE_CURVE('',#8240,#8230,#1213,.T.);
#10207=EDGE_CURVE('',#8240,#8239,#7071,.T.);
#10208=EDGE_CURVE('',#8241,#8240,#265,.T.);
#10209=EDGE_CURVE('',#8229,#8241,#1214,.T.);
#10210=EDGE_CURVE('',#8242,#8228,#1215,.T.);
#10211=EDGE_CURVE('',#8241,#8242,#1216,.T.);
#10212=EDGE_CURVE('',#8227,#8243,#1217,.T.);
#10213=EDGE_CURVE('',#8243,#8242,#266,.T.);
#10214=EDGE_CURVE('',#8237,#8244,#267,.T.);
#10215=EDGE_CURVE('',#8243,#8244,#7072,.T.);
#10216=EDGE_CURVE('',#8244,#8225,#1218,.T.);
#10217=EDGE_CURVE('',#8245,#8235,#1219,.T.);
#10218=EDGE_CURVE('',#8245,#8246,#1220,.T.);
#10219=EDGE_CURVE('',#8246,#8236,#1221,.T.);
#10220=EDGE_CURVE('',#8247,#8234,#1222,.T.);
#10221=EDGE_CURVE('',#8247,#8245,#7073,.T.);
#10222=EDGE_CURVE('',#8246,#8248,#7074,.T.);
#10223=EDGE_CURVE('',#8248,#8233,#1223,.T.);
#10224=EDGE_CURVE('',#8248,#8247,#1224,.T.);
#10225=EDGE_CURVE('',#8249,#8250,#268,.T.);
#10226=EDGE_CURVE('',#8249,#8251,#7075,.T.);
#10227=EDGE_CURVE('',#8252,#8251,#269,.T.);
#10228=EDGE_CURVE('',#8252,#8253,#1225,.T.);
#10229=EDGE_CURVE('',#8254,#8253,#270,.T.);
#10230=EDGE_CURVE('',#8255,#8254,#7076,.T.);
#10231=EDGE_CURVE('',#8256,#8255,#271,.T.);
#10232=EDGE_CURVE('',#8256,#8250,#1226,.T.);
#10233=EDGE_CURVE('',#8257,#8258,#1227,.T.);
#10234=EDGE_CURVE('',#8258,#8259,#208,.T.);
#10235=EDGE_CURVE('',#8259,#8260,#1228,.T.);
#10236=EDGE_CURVE('',#8260,#8257,#209,.T.);
#10237=EDGE_CURVE('',#8250,#8261,#1229,.T.);
#10238=EDGE_CURVE('',#8262,#8256,#1230,.T.);
#10239=EDGE_CURVE('',#8261,#8262,#1231,.T.);
#10240=EDGE_CURVE('',#8255,#8263,#1232,.T.);
#10241=EDGE_CURVE('',#8263,#8262,#272,.T.);
#10242=EDGE_CURVE('',#8264,#8254,#1233,.T.);
#10243=EDGE_CURVE('',#8264,#8263,#7077,.T.);
#10244=EDGE_CURVE('',#8265,#8264,#273,.T.);
#10245=EDGE_CURVE('',#8253,#8265,#1234,.T.);
#10246=EDGE_CURVE('',#8266,#8252,#1235,.T.);
#10247=EDGE_CURVE('',#8265,#8266,#1236,.T.);
#10248=EDGE_CURVE('',#8251,#8267,#1237,.T.);
#10249=EDGE_CURVE('',#8267,#8266,#274,.T.);
#10250=EDGE_CURVE('',#8261,#8268,#275,.T.);
#10251=EDGE_CURVE('',#8267,#8268,#7078,.T.);
#10252=EDGE_CURVE('',#8268,#8249,#1238,.T.);
#10253=EDGE_CURVE('',#8269,#8259,#1239,.T.);
#10254=EDGE_CURVE('',#8269,#8270,#1240,.T.);
#10255=EDGE_CURVE('',#8270,#8260,#1241,.T.);
#10256=EDGE_CURVE('',#8271,#8258,#1242,.T.);
#10257=EDGE_CURVE('',#8271,#8269,#7079,.T.);
#10258=EDGE_CURVE('',#8270,#8272,#7080,.T.);
#10259=EDGE_CURVE('',#8272,#8257,#1243,.T.);
#10260=EDGE_CURVE('',#8272,#8271,#1244,.T.);
#10261=EDGE_CURVE('',#8273,#8274,#276,.T.);
#10262=EDGE_CURVE('',#8273,#8275,#7081,.T.);
#10263=EDGE_CURVE('',#8276,#8275,#277,.T.);
#10264=EDGE_CURVE('',#8276,#8277,#1245,.T.);
#10265=EDGE_CURVE('',#8278,#8277,#278,.T.);
#10266=EDGE_CURVE('',#8279,#8278,#7082,.T.);
#10267=EDGE_CURVE('',#8280,#8279,#279,.T.);
#10268=EDGE_CURVE('',#8280,#8274,#1246,.T.);
#10269=EDGE_CURVE('',#8281,#8282,#1247,.T.);
#10270=EDGE_CURVE('',#8282,#8283,#210,.T.);
#10271=EDGE_CURVE('',#8283,#8284,#1248,.T.);
#10272=EDGE_CURVE('',#8284,#8281,#211,.T.);
#10273=EDGE_CURVE('',#8274,#8285,#1249,.T.);
#10274=EDGE_CURVE('',#8286,#8280,#1250,.T.);
#10275=EDGE_CURVE('',#8285,#8286,#1251,.T.);
#10276=EDGE_CURVE('',#8279,#8287,#1252,.T.);
#10277=EDGE_CURVE('',#8287,#8286,#280,.T.);
#10278=EDGE_CURVE('',#8288,#8278,#1253,.T.);
#10279=EDGE_CURVE('',#8288,#8287,#7083,.T.);
#10280=EDGE_CURVE('',#8289,#8288,#281,.T.);
#10281=EDGE_CURVE('',#8277,#8289,#1254,.T.);
#10282=EDGE_CURVE('',#8290,#8276,#1255,.T.);
#10283=EDGE_CURVE('',#8289,#8290,#1256,.T.);
#10284=EDGE_CURVE('',#8275,#8291,#1257,.T.);
#10285=EDGE_CURVE('',#8291,#8290,#282,.T.);
#10286=EDGE_CURVE('',#8285,#8292,#283,.T.);
#10287=EDGE_CURVE('',#8291,#8292,#7084,.T.);
#10288=EDGE_CURVE('',#8292,#8273,#1258,.T.);
#10289=EDGE_CURVE('',#8293,#8283,#1259,.T.);
#10290=EDGE_CURVE('',#8293,#8294,#1260,.T.);
#10291=EDGE_CURVE('',#8294,#8284,#1261,.T.);
#10292=EDGE_CURVE('',#8295,#8282,#1262,.T.);
#10293=EDGE_CURVE('',#8295,#8293,#7085,.T.);
#10294=EDGE_CURVE('',#8294,#8296,#7086,.T.);
#10295=EDGE_CURVE('',#8296,#8281,#1263,.T.);
#10296=EDGE_CURVE('',#8296,#8295,#1264,.T.);
#10297=EDGE_CURVE('',#8297,#8298,#284,.T.);
#10298=EDGE_CURVE('',#8297,#8299,#7087,.T.);
#10299=EDGE_CURVE('',#8300,#8299,#285,.T.);
#10300=EDGE_CURVE('',#8300,#8301,#1265,.T.);
#10301=EDGE_CURVE('',#8302,#8301,#286,.T.);
#10302=EDGE_CURVE('',#8303,#8302,#7088,.T.);
#10303=EDGE_CURVE('',#8304,#8303,#287,.T.);
#10304=EDGE_CURVE('',#8304,#8298,#1266,.T.);
#10305=EDGE_CURVE('',#8305,#8306,#1267,.T.);
#10306=EDGE_CURVE('',#8306,#8307,#212,.T.);
#10307=EDGE_CURVE('',#8307,#8308,#1268,.T.);
#10308=EDGE_CURVE('',#8308,#8305,#213,.T.);
#10309=EDGE_CURVE('',#8298,#8309,#1269,.T.);
#10310=EDGE_CURVE('',#8310,#8304,#1270,.T.);
#10311=EDGE_CURVE('',#8309,#8310,#1271,.T.);
#10312=EDGE_CURVE('',#8303,#8311,#1272,.T.);
#10313=EDGE_CURVE('',#8311,#8310,#288,.T.);
#10314=EDGE_CURVE('',#8312,#8302,#1273,.T.);
#10315=EDGE_CURVE('',#8312,#8311,#7089,.T.);
#10316=EDGE_CURVE('',#8313,#8312,#289,.T.);
#10317=EDGE_CURVE('',#8301,#8313,#1274,.T.);
#10318=EDGE_CURVE('',#8314,#8300,#1275,.T.);
#10319=EDGE_CURVE('',#8313,#8314,#1276,.T.);
#10320=EDGE_CURVE('',#8299,#8315,#1277,.T.);
#10321=EDGE_CURVE('',#8315,#8314,#290,.T.);
#10322=EDGE_CURVE('',#8309,#8316,#291,.T.);
#10323=EDGE_CURVE('',#8315,#8316,#7090,.T.);
#10324=EDGE_CURVE('',#8316,#8297,#1278,.T.);
#10325=EDGE_CURVE('',#8317,#8307,#1279,.T.);
#10326=EDGE_CURVE('',#8317,#8318,#1280,.T.);
#10327=EDGE_CURVE('',#8318,#8308,#1281,.T.);
#10328=EDGE_CURVE('',#8319,#8306,#1282,.T.);
#10329=EDGE_CURVE('',#8319,#8317,#7091,.T.);
#10330=EDGE_CURVE('',#8318,#8320,#7092,.T.);
#10331=EDGE_CURVE('',#8320,#8305,#1283,.T.);
#10332=EDGE_CURVE('',#8320,#8319,#1284,.T.);
#10333=EDGE_CURVE('',#8321,#8322,#292,.T.);
#10334=EDGE_CURVE('',#8321,#8323,#7093,.T.);
#10335=EDGE_CURVE('',#8324,#8323,#293,.T.);
#10336=EDGE_CURVE('',#8324,#8325,#1285,.T.);
#10337=EDGE_CURVE('',#8326,#8325,#294,.T.);
#10338=EDGE_CURVE('',#8327,#8326,#7094,.T.);
#10339=EDGE_CURVE('',#8328,#8327,#295,.T.);
#10340=EDGE_CURVE('',#8328,#8322,#1286,.T.);
#10341=EDGE_CURVE('',#8329,#8330,#1287,.T.);
#10342=EDGE_CURVE('',#8330,#8331,#214,.T.);
#10343=EDGE_CURVE('',#8331,#8332,#1288,.T.);
#10344=EDGE_CURVE('',#8332,#8329,#215,.T.);
#10345=EDGE_CURVE('',#8322,#8333,#1289,.T.);
#10346=EDGE_CURVE('',#8334,#8328,#1290,.T.);
#10347=EDGE_CURVE('',#8333,#8334,#1291,.T.);
#10348=EDGE_CURVE('',#8327,#8335,#1292,.T.);
#10349=EDGE_CURVE('',#8335,#8334,#296,.T.);
#10350=EDGE_CURVE('',#8336,#8326,#1293,.T.);
#10351=EDGE_CURVE('',#8336,#8335,#7095,.T.);
#10352=EDGE_CURVE('',#8337,#8336,#297,.T.);
#10353=EDGE_CURVE('',#8325,#8337,#1294,.T.);
#10354=EDGE_CURVE('',#8338,#8324,#1295,.T.);
#10355=EDGE_CURVE('',#8337,#8338,#1296,.T.);
#10356=EDGE_CURVE('',#8323,#8339,#1297,.T.);
#10357=EDGE_CURVE('',#8339,#8338,#298,.T.);
#10358=EDGE_CURVE('',#8333,#8340,#299,.T.);
#10359=EDGE_CURVE('',#8339,#8340,#7096,.T.);
#10360=EDGE_CURVE('',#8340,#8321,#1298,.T.);
#10361=EDGE_CURVE('',#8341,#8331,#1299,.T.);
#10362=EDGE_CURVE('',#8341,#8342,#1300,.T.);
#10363=EDGE_CURVE('',#8342,#8332,#1301,.T.);
#10364=EDGE_CURVE('',#8343,#8330,#1302,.T.);
#10365=EDGE_CURVE('',#8343,#8341,#7097,.T.);
#10366=EDGE_CURVE('',#8342,#8344,#7098,.T.);
#10367=EDGE_CURVE('',#8344,#8345,#7099,.T.);
#10368=EDGE_CURVE('',#8345,#8346,#7100,.T.);
#10369=EDGE_CURVE('',#8346,#8329,#1303,.T.);
#10370=EDGE_CURVE('',#8346,#8343,#1304,.T.);
#10371=EDGE_CURVE('',#8347,#8348,#1305,.T.);
#10372=EDGE_CURVE('',#8348,#8349,#1306,.T.);
#10373=EDGE_CURVE('',#8349,#8350,#1307,.T.);
#10374=EDGE_CURVE('',#8350,#8351,#1308,.T.);
#10375=EDGE_CURVE('',#8351,#8352,#1309,.T.);
#10376=EDGE_CURVE('',#8352,#8353,#1310,.T.);
#10377=EDGE_CURVE('',#8353,#8354,#1311,.T.);
#10378=EDGE_CURVE('',#8354,#8347,#1312,.T.);
#10379=EDGE_CURVE('',#8355,#8356,#1313,.T.);
#10380=EDGE_CURVE('',#8356,#8357,#1314,.T.);
#10381=EDGE_CURVE('',#8357,#8358,#1315,.T.);
#10382=EDGE_CURVE('',#8358,#8359,#1316,.T.);
#10383=EDGE_CURVE('',#8359,#8360,#1317,.T.);
#10384=EDGE_CURVE('',#8360,#8361,#1318,.T.);
#10385=EDGE_CURVE('',#8361,#8362,#1319,.T.);
#10386=EDGE_CURVE('',#8362,#8355,#1320,.T.);
#10387=EDGE_CURVE('',#8363,#8353,#1321,.T.);
#10388=EDGE_CURVE('',#8352,#8364,#1322,.T.);
#10389=EDGE_CURVE('',#8363,#8364,#1323,.T.);
#10390=EDGE_CURVE('',#8365,#8354,#1324,.T.);
#10391=EDGE_CURVE('',#8365,#8363,#1325,.T.);
#10392=EDGE_CURVE('',#8366,#8367,#1326,.T.);
#10393=EDGE_CURVE('',#8367,#8347,#1327,.T.);
#10394=EDGE_CURVE('',#8366,#8365,#1328,.T.);
#10395=EDGE_CURVE('',#8368,#8349,#1329,.T.);
#10396=EDGE_CURVE('',#8369,#8348,#1330,.T.);
#10397=EDGE_CURVE('',#8370,#8369,#1331,.T.);
#10398=EDGE_CURVE('',#8368,#8370,#1332,.T.);
#10399=EDGE_CURVE('',#8371,#8350,#1333,.T.);
#10400=EDGE_CURVE('',#8371,#8368,#1334,.T.);
#10401=EDGE_CURVE('',#8372,#8351,#1335,.T.);
#10402=EDGE_CURVE('',#8372,#8371,#1336,.T.);
#10403=EDGE_CURVE('',#8364,#8372,#1337,.T.);
#10404=EDGE_CURVE('',#8370,#8373,#1338,.T.);
#10405=EDGE_CURVE('',#8374,#8373,#1339,.T.);
#10406=EDGE_CURVE('',#8366,#8374,#1340,.T.);
#10407=EDGE_CURVE('',#8375,#8376,#1341,.T.);
#10408=EDGE_CURVE('',#8376,#8377,#1342,.T.);
#10409=EDGE_CURVE('',#8377,#8378,#1343,.T.);
#10410=EDGE_CURVE('',#8378,#8379,#1344,.T.);
#10411=EDGE_CURVE('',#8379,#8380,#1345,.T.);
#10412=EDGE_CURVE('',#8380,#8381,#1346,.T.);
#10413=EDGE_CURVE('',#8381,#8382,#1347,.T.);
#10414=EDGE_CURVE('',#8382,#8383,#1348,.T.);
#10415=EDGE_CURVE('',#8383,#8384,#1349,.T.);
#10416=EDGE_CURVE('',#8384,#8385,#1350,.T.);
#10417=EDGE_CURVE('',#8385,#8386,#1351,.T.);
#10418=EDGE_CURVE('',#8386,#8375,#1352,.T.);
#10419=EDGE_CURVE('',#8384,#8356,#1353,.T.);
#10420=EDGE_CURVE('',#8383,#8357,#1354,.T.);
#10421=EDGE_CURVE('',#8358,#8382,#1355,.T.);
#10422=EDGE_CURVE('',#8381,#8359,#1356,.T.);
#10423=EDGE_CURVE('',#8380,#8360,#1357,.T.);
#10424=EDGE_CURVE('',#8379,#8361,#1358,.T.);
#10425=EDGE_CURVE('',#8378,#8362,#1359,.T.);
#10426=EDGE_CURVE('',#8377,#8355,#1360,.T.);
#10427=EDGE_CURVE('',#8387,#8344,#1361,.T.);
#10428=EDGE_CURVE('',#8388,#8387,#1362,.T.);
#10429=EDGE_CURVE('',#8389,#8388,#1363,.T.);
#10430=EDGE_CURVE('',#8389,#8390,#1364,.T.);
#10431=EDGE_CURVE('',#8345,#8390,#1365,.T.);
#10432=EDGE_CURVE('',#8344,#8345,#1366,.T.);
#10433=EDGE_CURVE('',#8391,#8392,#1367,.T.);
#10434=EDGE_CURVE('',#8393,#8391,#1368,.T.);
#10435=EDGE_CURVE('',#8388,#8393,#1369,.T.);
#10436=EDGE_CURVE('',#8376,#8387,#1370,.T.);
#10437=EDGE_CURVE('',#8375,#8392,#1371,.T.);
#10438=EDGE_CURVE('',#8389,#8394,#1372,.T.);
#10439=EDGE_CURVE('',#8395,#8394,#1373,.T.);
#10440=EDGE_CURVE('',#8395,#8396,#1374,.T.);
#10441=EDGE_CURVE('',#8386,#8396,#1375,.T.);
#10442=EDGE_CURVE('',#8390,#8385,#1376,.T.);
#10443=EDGE_CURVE('',#8397,#8393,#1377,.T.);
#10444=EDGE_CURVE('',#8391,#8395,#1378,.T.);
#10445=EDGE_CURVE('',#8394,#8398,#1379,.T.);
#10446=EDGE_CURVE('',#8398,#8374,#1380,.T.);
#10447=EDGE_CURVE('',#8373,#8397,#1381,.T.);
#10448=EDGE_CURVE('',#8388,#8369,#1382,.T.);
#10449=EDGE_CURVE('',#8369,#8397,#1383,.T.);
#10450=EDGE_CURVE('',#8367,#8389,#1384,.T.);
#10451=EDGE_CURVE('',#8367,#8398,#1385,.T.);
#10452=EDGE_CURVE('',#8392,#8396,#1386,.T.);
#10453=EDGE_CURVE('',#8399,#8400,#1387,.T.);
#10454=EDGE_CURVE('',#8401,#8399,#7101,.T.);
#10455=EDGE_CURVE('',#8402,#8401,#1388,.T.);
#10456=EDGE_CURVE('',#8400,#8402,#7102,.T.);
#10457=EDGE_CURVE('',#8403,#8404,#1389,.T.);
#10458=EDGE_CURVE('',#8405,#8403,#7103,.T.);
#10459=EDGE_CURVE('',#8406,#8405,#1390,.T.);
#10460=EDGE_CURVE('',#8404,#8406,#7104,.T.);
#10461=EDGE_CURVE('',#8407,#8408,#1391,.T.);
#10462=EDGE_CURVE('',#8409,#8407,#7105,.T.);
#10463=EDGE_CURVE('',#8410,#8409,#1392,.T.);
#10464=EDGE_CURVE('',#8408,#8410,#7106,.T.);
#10465=EDGE_CURVE('',#8411,#8412,#1393,.T.);
#10466=EDGE_CURVE('',#8413,#8411,#7107,.T.);
#10467=EDGE_CURVE('',#8414,#8413,#1394,.T.);
#10468=EDGE_CURVE('',#8412,#8414,#7108,.T.);
#10469=EDGE_CURVE('',#8415,#8416,#1395,.T.);
#10470=EDGE_CURVE('',#8417,#8415,#7109,.T.);
#10471=EDGE_CURVE('',#8418,#8417,#1396,.T.);
#10472=EDGE_CURVE('',#8416,#8418,#7110,.T.);
#10473=EDGE_CURVE('',#8419,#8420,#1397,.T.);
#10474=EDGE_CURVE('',#8421,#8419,#7111,.T.);
#10475=EDGE_CURVE('',#8422,#8421,#1398,.T.);
#10476=EDGE_CURVE('',#8420,#8422,#7112,.T.);
#10477=EDGE_CURVE('',#8423,#8424,#1399,.T.);
#10478=EDGE_CURVE('',#8425,#8423,#7113,.T.);
#10479=EDGE_CURVE('',#8426,#8425,#1400,.T.);
#10480=EDGE_CURVE('',#8424,#8426,#7114,.T.);
#10481=EDGE_CURVE('',#8427,#8428,#1401,.T.);
#10482=EDGE_CURVE('',#8429,#8427,#7115,.T.);
#10483=EDGE_CURVE('',#8430,#8429,#1402,.T.);
#10484=EDGE_CURVE('',#8428,#8430,#7116,.T.);
#10485=EDGE_CURVE('',#8431,#8432,#1403,.T.);
#10486=EDGE_CURVE('',#8433,#8431,#7117,.T.);
#10487=EDGE_CURVE('',#8434,#8433,#1404,.T.);
#10488=EDGE_CURVE('',#8432,#8434,#7118,.T.);
#10489=EDGE_CURVE('',#8435,#8436,#1405,.T.);
#10490=EDGE_CURVE('',#8437,#8435,#7119,.T.);
#10491=EDGE_CURVE('',#8438,#8437,#1406,.T.);
#10492=EDGE_CURVE('',#8436,#8438,#7120,.T.);
#10493=EDGE_CURVE('',#8439,#8440,#1407,.T.);
#10494=EDGE_CURVE('',#8441,#8439,#7121,.T.);
#10495=EDGE_CURVE('',#8442,#8441,#1408,.T.);
#10496=EDGE_CURVE('',#8440,#8442,#7122,.T.);
#10497=EDGE_CURVE('',#8443,#8444,#1409,.T.);
#10498=EDGE_CURVE('',#8445,#8443,#7123,.T.);
#10499=EDGE_CURVE('',#8446,#8445,#1410,.T.);
#10500=EDGE_CURVE('',#8444,#8446,#7124,.T.);
#10501=EDGE_CURVE('',#8447,#8448,#1411,.T.);
#10502=EDGE_CURVE('',#8449,#8447,#7125,.T.);
#10503=EDGE_CURVE('',#8450,#8449,#1412,.T.);
#10504=EDGE_CURVE('',#8448,#8450,#7126,.T.);
#10505=EDGE_CURVE('',#8451,#8452,#1413,.T.);
#10506=EDGE_CURVE('',#8453,#8451,#7127,.T.);
#10507=EDGE_CURVE('',#8454,#8453,#1414,.T.);
#10508=EDGE_CURVE('',#8452,#8454,#7128,.T.);
#10509=EDGE_CURVE('',#8455,#8456,#1415,.T.);
#10510=EDGE_CURVE('',#8457,#8455,#7129,.T.);
#10511=EDGE_CURVE('',#8458,#8457,#1416,.T.);
#10512=EDGE_CURVE('',#8456,#8458,#7130,.T.);
#10513=EDGE_CURVE('',#8459,#8460,#1417,.T.);
#10514=EDGE_CURVE('',#8461,#8459,#7131,.T.);
#10515=EDGE_CURVE('',#8462,#8461,#1418,.T.);
#10516=EDGE_CURVE('',#8460,#8462,#7132,.T.);
#10517=EDGE_CURVE('',#8463,#8464,#1419,.T.);
#10518=EDGE_CURVE('',#8465,#8463,#7133,.T.);
#10519=EDGE_CURVE('',#8466,#8465,#1420,.T.);
#10520=EDGE_CURVE('',#8464,#8466,#7134,.T.);
#10521=EDGE_CURVE('',#8467,#8468,#1421,.T.);
#10522=EDGE_CURVE('',#8469,#8467,#7135,.T.);
#10523=EDGE_CURVE('',#8470,#8469,#1422,.T.);
#10524=EDGE_CURVE('',#8468,#8470,#7136,.T.);
#10525=EDGE_CURVE('',#8471,#8472,#1423,.T.);
#10526=EDGE_CURVE('',#8473,#8471,#7137,.T.);
#10527=EDGE_CURVE('',#8474,#8473,#1424,.T.);
#10528=EDGE_CURVE('',#8472,#8474,#7138,.T.);
#10529=EDGE_CURVE('',#8475,#8476,#1425,.T.);
#10530=EDGE_CURVE('',#8477,#8475,#7139,.T.);
#10531=EDGE_CURVE('',#8478,#8477,#1426,.T.);
#10532=EDGE_CURVE('',#8476,#8478,#7140,.T.);
#10533=EDGE_CURVE('',#8479,#8480,#1427,.T.);
#10534=EDGE_CURVE('',#8481,#8479,#7141,.T.);
#10535=EDGE_CURVE('',#8482,#8481,#1428,.T.);
#10536=EDGE_CURVE('',#8480,#8482,#7142,.T.);
#10537=EDGE_CURVE('',#8483,#8484,#1429,.T.);
#10538=EDGE_CURVE('',#8485,#8483,#7143,.T.);
#10539=EDGE_CURVE('',#8486,#8485,#1430,.T.);
#10540=EDGE_CURVE('',#8484,#8486,#7144,.T.);
#10541=EDGE_CURVE('',#8487,#8488,#1431,.T.);
#10542=EDGE_CURVE('',#8489,#8487,#7145,.T.);
#10543=EDGE_CURVE('',#8490,#8489,#1432,.T.);
#10544=EDGE_CURVE('',#8488,#8490,#7146,.T.);
#10545=EDGE_CURVE('',#8491,#8492,#1433,.T.);
#10546=EDGE_CURVE('',#8493,#8491,#7147,.T.);
#10547=EDGE_CURVE('',#8494,#8493,#1434,.T.);
#10548=EDGE_CURVE('',#8492,#8494,#7148,.T.);
#10549=EDGE_CURVE('',#8495,#8496,#1435,.T.);
#10550=EDGE_CURVE('',#8497,#8495,#7149,.T.);
#10551=EDGE_CURVE('',#8498,#8497,#1436,.T.);
#10552=EDGE_CURVE('',#8496,#8498,#7150,.T.);
#10553=EDGE_CURVE('',#8499,#8500,#1437,.T.);
#10554=EDGE_CURVE('',#8501,#8499,#7151,.T.);
#10555=EDGE_CURVE('',#8502,#8501,#1438,.T.);
#10556=EDGE_CURVE('',#8500,#8502,#7152,.T.);
#10557=EDGE_CURVE('',#8503,#8504,#1439,.T.);
#10558=EDGE_CURVE('',#8505,#8503,#7153,.T.);
#10559=EDGE_CURVE('',#8506,#8505,#1440,.T.);
#10560=EDGE_CURVE('',#8504,#8506,#7154,.T.);
#10561=EDGE_CURVE('',#8507,#8508,#1441,.T.);
#10562=EDGE_CURVE('',#8509,#8507,#7155,.T.);
#10563=EDGE_CURVE('',#8510,#8509,#1442,.T.);
#10564=EDGE_CURVE('',#8508,#8510,#7156,.T.);
#10565=EDGE_CURVE('',#8511,#8512,#1443,.T.);
#10566=EDGE_CURVE('',#8513,#8511,#7157,.T.);
#10567=EDGE_CURVE('',#8514,#8513,#1444,.T.);
#10568=EDGE_CURVE('',#8512,#8514,#7158,.T.);
#10569=EDGE_CURVE('',#8515,#8516,#1445,.T.);
#10570=EDGE_CURVE('',#8517,#8515,#7159,.T.);
#10571=EDGE_CURVE('',#8518,#8517,#1446,.T.);
#10572=EDGE_CURVE('',#8516,#8518,#7160,.T.);
#10573=EDGE_CURVE('',#8519,#8520,#1447,.T.);
#10574=EDGE_CURVE('',#8521,#8519,#7161,.T.);
#10575=EDGE_CURVE('',#8522,#8521,#1448,.T.);
#10576=EDGE_CURVE('',#8520,#8522,#7162,.T.);
#10577=EDGE_CURVE('',#8523,#8524,#1449,.T.);
#10578=EDGE_CURVE('',#8525,#8523,#7163,.T.);
#10579=EDGE_CURVE('',#8526,#8525,#1450,.T.);
#10580=EDGE_CURVE('',#8524,#8526,#7164,.T.);
#10581=EDGE_CURVE('',#8527,#8528,#1451,.T.);
#10582=EDGE_CURVE('',#8529,#8527,#7165,.T.);
#10583=EDGE_CURVE('',#8530,#8529,#1452,.T.);
#10584=EDGE_CURVE('',#8528,#8530,#7166,.T.);
#10585=EDGE_CURVE('',#8531,#8532,#1453,.T.);
#10586=EDGE_CURVE('',#8533,#8531,#7167,.T.);
#10587=EDGE_CURVE('',#8534,#8533,#1454,.T.);
#10588=EDGE_CURVE('',#8532,#8534,#7168,.T.);
#10589=EDGE_CURVE('',#8535,#8536,#1455,.T.);
#10590=EDGE_CURVE('',#8537,#8535,#7169,.T.);
#10591=EDGE_CURVE('',#8538,#8537,#1456,.T.);
#10592=EDGE_CURVE('',#8536,#8538,#7170,.T.);
#10593=EDGE_CURVE('',#8539,#8540,#1457,.T.);
#10594=EDGE_CURVE('',#8541,#8539,#7171,.T.);
#10595=EDGE_CURVE('',#8542,#8541,#1458,.T.);
#10596=EDGE_CURVE('',#8540,#8542,#7172,.T.);
#10597=EDGE_CURVE('',#8543,#8544,#1459,.T.);
#10598=EDGE_CURVE('',#8545,#8543,#7173,.T.);
#10599=EDGE_CURVE('',#8546,#8545,#1460,.T.);
#10600=EDGE_CURVE('',#8544,#8546,#7174,.T.);
#10601=EDGE_CURVE('',#8547,#8548,#1461,.T.);
#10602=EDGE_CURVE('',#8549,#8547,#7175,.T.);
#10603=EDGE_CURVE('',#8550,#8549,#1462,.T.);
#10604=EDGE_CURVE('',#8548,#8550,#7176,.T.);
#10605=EDGE_CURVE('',#8551,#8552,#1463,.T.);
#10606=EDGE_CURVE('',#8553,#8551,#7177,.T.);
#10607=EDGE_CURVE('',#8554,#8553,#1464,.T.);
#10608=EDGE_CURVE('',#8552,#8554,#7178,.T.);
#10609=EDGE_CURVE('',#8555,#8556,#1465,.T.);
#10610=EDGE_CURVE('',#8557,#8555,#7179,.T.);
#10611=EDGE_CURVE('',#8558,#8557,#1466,.T.);
#10612=EDGE_CURVE('',#8556,#8558,#7180,.T.);
#10613=EDGE_CURVE('',#8559,#8560,#1467,.T.);
#10614=EDGE_CURVE('',#8561,#8559,#7181,.T.);
#10615=EDGE_CURVE('',#8562,#8561,#1468,.T.);
#10616=EDGE_CURVE('',#8560,#8562,#7182,.T.);
#10617=EDGE_CURVE('',#8563,#8564,#1469,.T.);
#10618=EDGE_CURVE('',#8565,#8563,#7183,.T.);
#10619=EDGE_CURVE('',#8566,#8565,#1470,.T.);
#10620=EDGE_CURVE('',#8564,#8566,#7184,.T.);
#10621=EDGE_CURVE('',#8567,#8568,#1471,.T.);
#10622=EDGE_CURVE('',#8569,#8567,#7185,.T.);
#10623=EDGE_CURVE('',#8570,#8569,#1472,.T.);
#10624=EDGE_CURVE('',#8568,#8570,#7186,.T.);
#10625=EDGE_CURVE('',#8571,#8572,#1473,.T.);
#10626=EDGE_CURVE('',#8573,#8571,#7187,.T.);
#10627=EDGE_CURVE('',#8574,#8573,#1474,.T.);
#10628=EDGE_CURVE('',#8572,#8574,#7188,.T.);
#10629=EDGE_CURVE('',#8402,#8575,#7189,.T.);
#10630=EDGE_CURVE('',#8575,#8576,#7190,.T.);
#10631=EDGE_CURVE('',#8576,#8572,#7191,.T.);
#10632=EDGE_CURVE('',#8574,#8568,#7192,.T.);
#10633=EDGE_CURVE('',#8570,#8564,#7193,.T.);
#10634=EDGE_CURVE('',#8566,#8560,#7194,.T.);
#10635=EDGE_CURVE('',#8562,#8556,#7195,.T.);
#10636=EDGE_CURVE('',#8558,#8552,#7196,.T.);
#10637=EDGE_CURVE('',#8554,#8548,#7197,.T.);
#10638=EDGE_CURVE('',#8550,#8544,#7198,.T.);
#10639=EDGE_CURVE('',#8546,#8540,#7199,.T.);
#10640=EDGE_CURVE('',#8542,#8536,#7200,.T.);
#10641=EDGE_CURVE('',#8538,#8532,#7201,.T.);
#10642=EDGE_CURVE('',#8534,#8528,#7202,.T.);
#10643=EDGE_CURVE('',#8530,#8524,#7203,.T.);
#10644=EDGE_CURVE('',#8526,#8520,#7204,.T.);
#10645=EDGE_CURVE('',#8522,#8516,#7205,.T.);
#10646=EDGE_CURVE('',#8518,#8512,#7206,.T.);
#10647=EDGE_CURVE('',#8514,#8508,#7207,.T.);
#10648=EDGE_CURVE('',#8510,#8504,#7208,.T.);
#10649=EDGE_CURVE('',#8506,#8500,#7209,.T.);
#10650=EDGE_CURVE('',#8502,#8496,#7210,.T.);
#10651=EDGE_CURVE('',#8498,#8492,#7211,.T.);
#10652=EDGE_CURVE('',#8494,#8488,#7212,.T.);
#10653=EDGE_CURVE('',#8490,#8484,#7213,.T.);
#10654=EDGE_CURVE('',#8486,#8480,#7214,.T.);
#10655=EDGE_CURVE('',#8482,#8476,#7215,.T.);
#10656=EDGE_CURVE('',#8478,#8472,#7216,.T.);
#10657=EDGE_CURVE('',#8474,#8468,#7217,.T.);
#10658=EDGE_CURVE('',#8470,#8464,#7218,.T.);
#10659=EDGE_CURVE('',#8466,#8460,#7219,.T.);
#10660=EDGE_CURVE('',#8462,#8456,#7220,.T.);
#10661=EDGE_CURVE('',#8458,#8452,#7221,.T.);
#10662=EDGE_CURVE('',#8454,#8448,#7222,.T.);
#10663=EDGE_CURVE('',#8450,#8444,#7223,.T.);
#10664=EDGE_CURVE('',#8446,#8440,#7224,.T.);
#10665=EDGE_CURVE('',#8442,#8436,#7225,.T.);
#10666=EDGE_CURVE('',#8438,#8432,#7226,.T.);
#10667=EDGE_CURVE('',#8434,#8428,#7227,.T.);
#10668=EDGE_CURVE('',#8430,#8424,#7228,.T.);
#10669=EDGE_CURVE('',#8426,#8420,#7229,.T.);
#10670=EDGE_CURVE('',#8422,#8416,#7230,.T.);
#10671=EDGE_CURVE('',#8418,#8412,#7231,.T.);
#10672=EDGE_CURVE('',#8414,#8408,#7232,.T.);
#10673=EDGE_CURVE('',#8410,#8404,#7233,.T.);
#10674=EDGE_CURVE('',#8406,#8400,#7234,.T.);
#10675=EDGE_CURVE('',#8577,#8577,#7235,.T.);
#10676=EDGE_CURVE('',#8578,#8401,#7236,.T.);
#10677=EDGE_CURVE('',#8578,#8575,#1475,.T.);
#10678=EDGE_CURVE('',#8576,#8579,#1476,.T.);
#10679=EDGE_CURVE('',#8571,#8579,#7237,.T.);
#10680=EDGE_CURVE('',#8567,#8573,#7238,.T.);
#10681=EDGE_CURVE('',#8563,#8569,#7239,.T.);
#10682=EDGE_CURVE('',#8559,#8565,#7240,.T.);
#10683=EDGE_CURVE('',#8555,#8561,#7241,.T.);
#10684=EDGE_CURVE('',#8551,#8557,#7242,.T.);
#10685=EDGE_CURVE('',#8547,#8553,#7243,.T.);
#10686=EDGE_CURVE('',#8543,#8549,#7244,.T.);
#10687=EDGE_CURVE('',#8539,#8545,#7245,.T.);
#10688=EDGE_CURVE('',#8535,#8541,#7246,.T.);
#10689=EDGE_CURVE('',#8531,#8537,#7247,.T.);
#10690=EDGE_CURVE('',#8527,#8533,#7248,.T.);
#10691=EDGE_CURVE('',#8523,#8529,#7249,.T.);
#10692=EDGE_CURVE('',#8519,#8525,#7250,.T.);
#10693=EDGE_CURVE('',#8515,#8521,#7251,.T.);
#10694=EDGE_CURVE('',#8511,#8517,#7252,.T.);
#10695=EDGE_CURVE('',#8507,#8513,#7253,.T.);
#10696=EDGE_CURVE('',#8503,#8509,#7254,.T.);
#10697=EDGE_CURVE('',#8499,#8505,#7255,.T.);
#10698=EDGE_CURVE('',#8495,#8501,#7256,.T.);
#10699=EDGE_CURVE('',#8491,#8497,#7257,.T.);
#10700=EDGE_CURVE('',#8487,#8493,#7258,.T.);
#10701=EDGE_CURVE('',#8483,#8489,#7259,.T.);
#10702=EDGE_CURVE('',#8479,#8485,#7260,.T.);
#10703=EDGE_CURVE('',#8475,#8481,#7261,.T.);
#10704=EDGE_CURVE('',#8471,#8477,#7262,.T.);
#10705=EDGE_CURVE('',#8467,#8473,#7263,.T.);
#10706=EDGE_CURVE('',#8463,#8469,#7264,.T.);
#10707=EDGE_CURVE('',#8459,#8465,#7265,.T.);
#10708=EDGE_CURVE('',#8455,#8461,#7266,.T.);
#10709=EDGE_CURVE('',#8451,#8457,#7267,.T.);
#10710=EDGE_CURVE('',#8447,#8453,#7268,.T.);
#10711=EDGE_CURVE('',#8443,#8449,#7269,.T.);
#10712=EDGE_CURVE('',#8439,#8445,#7270,.T.);
#10713=EDGE_CURVE('',#8435,#8441,#7271,.T.);
#10714=EDGE_CURVE('',#8431,#8437,#7272,.T.);
#10715=EDGE_CURVE('',#8427,#8433,#7273,.T.);
#10716=EDGE_CURVE('',#8423,#8429,#7274,.T.);
#10717=EDGE_CURVE('',#8419,#8425,#7275,.T.);
#10718=EDGE_CURVE('',#8415,#8421,#7276,.T.);
#10719=EDGE_CURVE('',#8411,#8417,#7277,.T.);
#10720=EDGE_CURVE('',#8407,#8413,#7278,.T.);
#10721=EDGE_CURVE('',#8403,#8409,#7279,.T.);
#10722=EDGE_CURVE('',#8579,#8578,#7280,.T.);
#10723=EDGE_CURVE('',#8399,#8405,#7281,.T.);
#10724=EDGE_CURVE('',#8580,#8580,#7282,.T.);
#10725=EDGE_CURVE('',#8580,#8577,#1477,.T.);
#10726=EDGE_CURVE('',#8581,#8582,#1478,.T.);
#10727=EDGE_CURVE('',#8583,#8581,#1479,.T.);
#10728=EDGE_CURVE('',#8584,#8583,#1480,.T.);
#10729=EDGE_CURVE('',#8584,#8582,#1481,.T.);
#10730=EDGE_CURVE('',#8582,#8585,#300,.T.);
#10731=EDGE_CURVE('',#8586,#8584,#7283,.T.);
#10732=EDGE_CURVE('',#8586,#8587,#1482,.T.);
#10733=EDGE_CURVE('',#8585,#8587,#301,.T.);
#10734=EDGE_CURVE('',#8587,#8588,#302,.T.);
#10735=EDGE_CURVE('',#8589,#8586,#7284,.T.);
#10736=EDGE_CURVE('',#8589,#8590,#1483,.T.);
#10737=EDGE_CURVE('',#8591,#8590,#303,.T.);
#10738=EDGE_CURVE('',#8592,#8591,#7285,.T.);
#10739=EDGE_CURVE('',#8593,#8592,#216,.T.);
#10740=EDGE_CURVE('',#8588,#8593,#7286,.T.);
#10741=EDGE_CURVE('',#8590,#8594,#304,.T.);
#10742=EDGE_CURVE('',#8595,#8589,#7287,.T.);
#10743=EDGE_CURVE('',#8595,#8596,#1484,.T.);
#10744=EDGE_CURVE('',#8594,#8596,#305,.T.);
#10745=EDGE_CURVE('',#8596,#8597,#1485,.T.);
#10746=EDGE_CURVE('',#8598,#8595,#1486,.T.);
#10747=EDGE_CURVE('',#8598,#8597,#1487,.T.);
#10748=EDGE_CURVE('',#8597,#8599,#306,.T.);
#10749=EDGE_CURVE('',#8600,#8598,#7288,.T.);
#10750=EDGE_CURVE('',#8600,#8601,#1488,.T.);
#10751=EDGE_CURVE('',#8599,#8601,#307,.T.);
#10752=EDGE_CURVE('',#8601,#8602,#308,.T.);
#10753=EDGE_CURVE('',#8603,#8600,#7289,.T.);
#10754=EDGE_CURVE('',#8603,#8604,#1489,.T.);
#10755=EDGE_CURVE('',#8605,#8604,#309,.T.);
#10756=EDGE_CURVE('',#8606,#8605,#7290,.T.);
#10757=EDGE_CURVE('',#8607,#8606,#217,.T.);
#10758=EDGE_CURVE('',#8602,#8607,#7291,.T.);
#10759=EDGE_CURVE('',#8604,#8608,#310,.T.);
#10760=EDGE_CURVE('',#8609,#8603,#7292,.T.);
#10761=EDGE_CURVE('',#8609,#8610,#1490,.T.);
#10762=EDGE_CURVE('',#8608,#8610,#311,.T.);
#10763=EDGE_CURVE('',#8610,#8611,#1491,.T.);
#10764=EDGE_CURVE('',#8612,#8609,#1492,.T.);
#10765=EDGE_CURVE('',#8612,#8611,#1493,.T.);
#10766=EDGE_CURVE('',#8611,#8613,#312,.T.);
#10767=EDGE_CURVE('',#8614,#8612,#7293,.T.);
#10768=EDGE_CURVE('',#8614,#8615,#1494,.T.);
#10769=EDGE_CURVE('',#8613,#8615,#313,.T.);
#10770=EDGE_CURVE('',#8615,#8616,#314,.T.);
#10771=EDGE_CURVE('',#8617,#8614,#7294,.T.);
#10772=EDGE_CURVE('',#8617,#8618,#1495,.T.);
#10773=EDGE_CURVE('',#8619,#8618,#315,.T.);
#10774=EDGE_CURVE('',#8620,#8619,#7295,.T.);
#10775=EDGE_CURVE('',#8621,#8620,#218,.T.);
#10776=EDGE_CURVE('',#8616,#8621,#7296,.T.);
#10777=EDGE_CURVE('',#8622,#8623,#1496,.T.);
#10778=EDGE_CURVE('',#8622,#8624,#1497,.T.);
#10779=EDGE_CURVE('',#8625,#8624,#1498,.T.);
#10780=EDGE_CURVE('',#8623,#8625,#1499,.T.);
#10781=EDGE_CURVE('',#8626,#8627,#1500,.T.);
#10782=EDGE_CURVE('',#8628,#8626,#1501,.T.);
#10783=EDGE_CURVE('',#8629,#8628,#1502,.T.);
#10784=EDGE_CURVE('',#8629,#8627,#1503,.T.);
#10785=EDGE_CURVE('',#8627,#8630,#1504,.T.);
#10786=EDGE_CURVE('',#8631,#8629,#1505,.T.);
#10787=EDGE_CURVE('',#8632,#8631,#1506,.T.);
#10788=EDGE_CURVE('',#8630,#8632,#1507,.T.);
#10789=EDGE_CURVE('',#8633,#8634,#1508,.T.);
#10790=EDGE_CURVE('',#8635,#8633,#1509,.T.);
#10791=EDGE_CURVE('',#8636,#8635,#1510,.T.);
#10792=EDGE_CURVE('',#8636,#8634,#1511,.T.);
#10793=EDGE_CURVE('',#8637,#8638,#316,.T.);
#10794=EDGE_CURVE('',#8634,#8637,#317,.T.);
#10795=EDGE_CURVE('',#8639,#8636,#7297,.T.);
#10796=EDGE_CURVE('',#8639,#8638,#1512,.T.);
#10797=EDGE_CURVE('',#8640,#8641,#318,.T.);
#10798=EDGE_CURVE('',#8642,#8640,#7298,.T.);
#10799=EDGE_CURVE('',#8643,#8642,#219,.T.);
#10800=EDGE_CURVE('',#8644,#8643,#7299,.T.);
#10801=EDGE_CURVE('',#8638,#8644,#319,.T.);
#10802=EDGE_CURVE('',#8645,#8639,#7300,.T.);
#10803=EDGE_CURVE('',#8645,#8641,#1513,.T.);
#10804=EDGE_CURVE('',#8646,#8581,#320,.T.);
#10805=EDGE_CURVE('',#8641,#8646,#321,.T.);
#10806=EDGE_CURVE('',#8583,#8645,#7301,.T.);
#10807=EDGE_CURVE('',#8647,#8617,#7302,.T.);
#10808=EDGE_CURVE('',#8647,#8648,#1514,.T.);
#10809=EDGE_CURVE('',#8649,#8648,#322,.T.);
#10810=EDGE_CURVE('',#8618,#8649,#323,.T.);
#10811=EDGE_CURVE('',#8650,#8647,#1515,.T.);
#10812=EDGE_CURVE('',#8651,#8650,#1516,.T.);
#10813=EDGE_CURVE('',#8648,#8651,#1517,.T.);
#10814=EDGE_CURVE('',#8652,#8622,#1518,.T.);
#10815=EDGE_CURVE('',#8653,#8652,#1519,.T.);
#10816=EDGE_CURVE('',#8654,#8653,#1520,.T.);
#10817=EDGE_CURVE('',#8624,#8654,#1521,.T.);
#10818=EDGE_CURVE('',#8646,#8585,#1522,.T.);
#10819=EDGE_CURVE('',#8655,#8656,#7303,.T.);
#10820=EDGE_CURVE('',#8656,#8657,#1523,.T.);
#10821=EDGE_CURVE('',#8657,#8593,#7304,.T.);
#10822=EDGE_CURVE('',#8592,#8657,#7305,.T.);
#10823=EDGE_CURVE('',#8656,#8655,#7306,.T.);
#10824=EDGE_CURVE('',#8594,#8599,#1524,.T.);
#10825=EDGE_CURVE('',#8602,#8591,#1525,.T.);
#10826=EDGE_CURVE('',#8658,#8659,#7307,.T.);
#10827=EDGE_CURVE('',#8659,#8660,#1526,.T.);
#10828=EDGE_CURVE('',#8660,#8607,#7308,.T.);
#10829=EDGE_CURVE('',#8606,#8660,#7309,.T.);
#10830=EDGE_CURVE('',#8659,#8658,#7310,.T.);
#10831=EDGE_CURVE('',#8608,#8613,#1527,.T.);
#10832=EDGE_CURVE('',#8616,#8605,#1528,.T.);
#10833=EDGE_CURVE('',#8661,#8662,#7311,.T.);
#10834=EDGE_CURVE('',#8662,#8663,#1529,.T.);
#10835=EDGE_CURVE('',#8663,#8621,#7312,.T.);
#10836=EDGE_CURVE('',#8620,#8663,#7313,.T.);
#10837=EDGE_CURVE('',#8662,#8661,#7314,.T.);
#10838=EDGE_CURVE('',#8664,#8649,#1530,.T.);
#10839=EDGE_CURVE('',#8665,#8664,#1531,.T.);
#10840=EDGE_CURVE('',#8665,#8619,#1532,.T.);
#10841=EDGE_CURVE('',#8666,#8625,#1533,.T.);
#10842=EDGE_CURVE('',#8667,#8666,#1534,.T.);
#10843=EDGE_CURVE('',#8667,#8623,#1535,.T.);
#10844=EDGE_CURVE('',#8654,#8668,#1536,.T.);
#10845=EDGE_CURVE('',#8668,#8665,#1537,.T.);
#10846=EDGE_CURVE('',#8664,#8666,#1538,.T.);
#10847=EDGE_CURVE('',#8632,#8669,#1539,.T.);
#10848=EDGE_CURVE('',#8669,#8670,#1540,.T.);
#10849=EDGE_CURVE('',#8670,#8630,#1541,.T.);
#10850=EDGE_CURVE('',#8588,#8640,#1542,.T.);
#10851=EDGE_CURVE('',#8671,#8668,#1543,.T.);
#10852=EDGE_CURVE('',#8672,#8671,#1544,.T.);
#10853=EDGE_CURVE('',#8644,#8672,#1545,.T.);
#10854=EDGE_CURVE('',#8673,#8643,#7315,.T.);
#10855=EDGE_CURVE('',#8642,#8673,#7316,.T.);
#10856=EDGE_CURVE('',#8674,#8674,#7317,.T.);
#10857=EDGE_CURVE('',#8675,#8675,#7318,.T.);
#10858=EDGE_CURVE('',#8675,#8658,#1546,.T.);
#10859=EDGE_CURVE('',#8676,#8676,#7319,.T.);
#10860=EDGE_CURVE('',#8676,#8661,#1547,.T.);
#10861=EDGE_CURVE('',#8677,#8678,#7320,.T.);
#10862=EDGE_CURVE('',#8678,#8673,#1548,.T.);
#10863=EDGE_CURVE('',#8678,#8677,#7321,.T.);
#10864=EDGE_CURVE('',#8679,#8679,#7322,.T.);
#10865=EDGE_CURVE('',#8679,#8677,#1549,.T.);
#10866=EDGE_CURVE('',#8680,#8680,#7323,.T.);
#10867=EDGE_CURVE('',#8680,#8655,#1550,.T.);
#10868=EDGE_CURVE('',#8681,#8682,#7324,.T.);
#10869=EDGE_CURVE('',#8682,#8683,#1551,.T.);
#10870=EDGE_CURVE('',#8683,#8684,#7325,.T.);
#10871=EDGE_CURVE('',#8684,#8681,#1552,.T.);
#10872=EDGE_CURVE('',#8685,#8633,#1553,.T.);
#10873=EDGE_CURVE('',#8685,#8683,#1554,.T.);
#10874=EDGE_CURVE('',#8635,#8682,#1555,.T.);
#10875=EDGE_CURVE('',#8681,#8686,#1556,.T.);
#10876=EDGE_CURVE('',#8686,#8687,#1557,.T.);
#10877=EDGE_CURVE('',#8687,#8688,#1558,.T.);
#10878=EDGE_CURVE('',#8688,#8689,#1559,.T.);
#10879=EDGE_CURVE('',#8689,#8690,#1560,.T.);
#10880=EDGE_CURVE('',#8690,#8691,#1561,.T.);
#10881=EDGE_CURVE('',#8691,#8692,#1562,.T.);
#10882=EDGE_CURVE('',#8693,#8692,#7326,.T.);
#10883=EDGE_CURVE('',#8693,#8650,#1563,.T.);
#10884=EDGE_CURVE('',#8694,#8694,#7327,.T.);
#10885=EDGE_CURVE('',#8695,#8695,#7328,.T.);
#10886=EDGE_CURVE('',#8696,#8696,#7329,.T.);
#10887=EDGE_CURVE('',#8697,#8697,#7330,.T.);
#10888=EDGE_CURVE('',#8692,#8698,#1564,.T.);
#10889=EDGE_CURVE('',#8698,#8699,#7331,.T.);
#10890=EDGE_CURVE('',#8699,#8693,#1565,.T.);
#10891=EDGE_CURVE('',#8691,#8700,#1566,.T.);
#10892=EDGE_CURVE('',#8700,#8701,#1567,.T.);
#10893=EDGE_CURVE('',#8701,#8702,#1568,.T.);
#10894=EDGE_CURVE('',#8702,#8703,#1569,.T.);
#10895=EDGE_CURVE('',#8703,#8704,#1570,.T.);
#10896=EDGE_CURVE('',#8704,#8698,#1571,.T.);
#10897=EDGE_CURVE('',#8699,#8667,#1572,.T.);
#10898=EDGE_CURVE('',#8651,#8667,#1573,.T.);
#10899=EDGE_CURVE('',#8671,#8631,#1574,.T.);
#10900=EDGE_CURVE('',#8669,#8671,#1575,.T.);
#10901=EDGE_CURVE('',#8705,#8653,#1576,.T.);
#10902=EDGE_CURVE('',#8668,#8705,#1577,.T.);
#10903=EDGE_CURVE('',#8652,#8706,#1578,.T.);
#10904=EDGE_CURVE('',#8706,#8705,#1579,.T.);
#10905=EDGE_CURVE('',#8705,#8669,#1580,.T.);
#10906=EDGE_CURVE('',#8628,#8707,#1581,.T.);
#10907=EDGE_CURVE('',#8708,#8707,#1582,.T.);
#10908=EDGE_CURVE('',#8672,#8708,#1583,.T.);
#10909=EDGE_CURVE('',#8709,#8710,#7332,.T.);
#10910=EDGE_CURVE('',#8709,#8711,#1584,.T.);
#10911=EDGE_CURVE('',#8711,#8712,#7333,.T.);
#10912=EDGE_CURVE('',#8712,#8710,#1585,.T.);
#10913=EDGE_CURVE('',#8709,#8713,#1586,.T.);
#10914=EDGE_CURVE('',#8714,#8713,#1587,.T.);
#10915=EDGE_CURVE('',#8711,#8714,#1588,.T.);
#10916=EDGE_CURVE('',#8715,#8713,#7334,.T.);
#10917=EDGE_CURVE('',#8715,#8716,#1589,.T.);
#10918=EDGE_CURVE('',#8716,#8714,#7335,.T.);
#10919=EDGE_CURVE('',#8715,#8717,#1590,.T.);
#10920=EDGE_CURVE('',#8718,#8717,#1591,.T.);
#10921=EDGE_CURVE('',#8716,#8718,#1592,.T.);
#10922=EDGE_CURVE('',#8719,#8717,#7336,.T.);
#10923=EDGE_CURVE('',#8719,#8720,#1593,.T.);
#10924=EDGE_CURVE('',#8720,#8718,#7337,.T.);
#10925=EDGE_CURVE('',#8719,#8721,#1594,.T.);
#10926=EDGE_CURVE('',#8722,#8721,#1595,.T.);
#10927=EDGE_CURVE('',#8720,#8722,#1596,.T.);
#10928=EDGE_CURVE('',#8723,#8721,#7338,.T.);
#10929=EDGE_CURVE('',#8723,#8724,#1597,.T.);
#10930=EDGE_CURVE('',#8724,#8722,#7339,.T.);
#10931=EDGE_CURVE('',#8723,#8710,#1598,.T.);
#10932=EDGE_CURVE('',#8724,#8712,#1599,.T.);
#10933=EDGE_CURVE('',#8708,#8637,#1600,.T.);
#10934=EDGE_CURVE('',#8725,#8725,#7340,.T.);
#10935=EDGE_CURVE('',#8725,#8674,#1601,.T.);
#10936=EDGE_CURVE('',#8626,#8685,#1602,.T.);
#10937=EDGE_CURVE('',#8707,#8685,#1603,.T.);
#10938=EDGE_CURVE('',#8706,#8670,#1604,.T.);
#10939=EDGE_CURVE('',#8726,#8727,#7341,.T.);
#10940=EDGE_CURVE('',#8728,#8726,#1605,.T.);
#10941=EDGE_CURVE('',#8729,#8728,#7342,.T.);
#10942=EDGE_CURVE('',#8727,#8729,#1606,.T.);
#10943=EDGE_CURVE('',#8729,#8728,#1607,.T.);
#10944=EDGE_CURVE('',#8704,#8701,#7343,.T.);
#10945=EDGE_CURVE('',#8702,#8703,#7344,.T.);
#10946=EDGE_CURVE('',#8730,#8731,#7345,.T.);
#10947=EDGE_CURVE('',#8732,#8730,#1608,.T.);
#10948=EDGE_CURVE('',#8733,#8732,#7346,.T.);
#10949=EDGE_CURVE('',#8731,#8733,#1609,.T.);
#10950=EDGE_CURVE('',#8733,#8732,#1610,.T.);
#10951=EDGE_CURVE('',#8684,#8727,#1611,.T.);
#10952=EDGE_CURVE('',#8726,#8734,#1612,.T.);
#10953=EDGE_CURVE('',#8686,#8734,#1613,.T.);
#10954=EDGE_CURVE('',#8730,#8735,#1614,.T.);
#10955=EDGE_CURVE('',#8690,#8735,#1615,.T.);
#10956=EDGE_CURVE('',#8689,#8736,#1616,.T.);
#10957=EDGE_CURVE('',#8736,#8731,#1617,.T.);
#10958=EDGE_CURVE('',#8737,#8738,#7347,.T.);
#10959=EDGE_CURVE('',#8739,#8737,#1618,.T.);
#10960=EDGE_CURVE('',#8740,#8739,#7348,.T.);
#10961=EDGE_CURVE('',#8738,#8740,#1619,.T.);
#10962=EDGE_CURVE('',#8740,#8739,#1620,.T.);
#10963=EDGE_CURVE('',#8737,#8741,#1621,.T.);
#10964=EDGE_CURVE('',#8688,#8741,#1622,.T.);
#10965=EDGE_CURVE('',#8687,#8742,#1623,.T.);
#10966=EDGE_CURVE('',#8742,#8738,#1624,.T.);
#10967=EDGE_CURVE('',#8743,#8743,#7349,.T.);
#10968=EDGE_CURVE('',#8743,#8744,#1625,.T.);
#10969=EDGE_CURVE('',#8744,#8744,#7350,.T.);
#10970=EDGE_CURVE('',#8745,#8745,#7351,.T.);
#10971=EDGE_CURVE('',#8746,#8746,#7352,.T.);
#10972=EDGE_CURVE('',#8746,#8743,#1626,.T.);
#10973=EDGE_CURVE('',#8747,#8748,#7353,.T.);
#10974=EDGE_CURVE('',#8748,#8745,#1627,.T.);
#10975=EDGE_CURVE('',#8748,#8747,#7354,.T.);
#10976=EDGE_CURVE('',#8747,#8749,#1628,.T.);
#10977=EDGE_CURVE('',#8749,#8749,#7355,.T.);
#10978=EDGE_CURVE('',#8750,#8750,#7356,.T.);
#10979=EDGE_CURVE('',#8694,#8750,#1629,.T.);
#10980=EDGE_CURVE('',#8751,#8751,#7357,.T.);
#10981=EDGE_CURVE('',#8695,#8751,#1630,.T.);
#10982=EDGE_CURVE('',#8752,#8752,#7358,.T.);
#10983=EDGE_CURVE('',#8696,#8752,#1631,.T.);
#10984=EDGE_CURVE('',#8753,#8753,#7359,.T.);
#10985=EDGE_CURVE('',#8697,#8753,#1632,.T.);
#10986=EDGE_CURVE('',#8735,#8700,#1633,.T.);
#10987=EDGE_CURVE('',#8741,#8736,#1634,.T.);
#10988=EDGE_CURVE('',#8734,#8742,#1635,.T.);
#10989=EDGE_CURVE('',#8754,#8754,#7360,.T.);
#10990=EDGE_CURVE('',#8754,#8755,#1636,.T.);
#10991=EDGE_CURVE('',#8755,#8755,#7361,.T.);
#10992=EDGE_CURVE('',#8756,#8756,#7362,.T.);
#10993=EDGE_CURVE('',#8756,#8757,#7363,.T.);
#10994=EDGE_CURVE('',#8757,#8758,#7364,.T.);
#10995=EDGE_CURVE('',#8758,#8757,#7365,.T.);
#10996=EDGE_CURVE('',#8758,#8759,#1637,.T.);
#10997=EDGE_CURVE('',#8760,#8759,#7366,.T.);
#10998=EDGE_CURVE('',#8759,#8760,#7367,.T.);
#10999=EDGE_CURVE('',#8761,#8761,#7368,.T.);
#11000=EDGE_CURVE('',#8760,#8762,#7369,.T.);
#11001=EDGE_CURVE('',#8762,#8762,#7370,.T.);
#11002=EDGE_CURVE('',#8763,#8763,#7371,.T.);
#11003=EDGE_CURVE('',#8763,#8761,#1638,.T.);
#11004=EDGE_CURVE('',#8764,#8765,#1639,.T.);
#11005=EDGE_CURVE('',#8766,#8765,#1640,.T.);
#11006=EDGE_CURVE('',#8766,#8767,#1641,.T.);
#11007=EDGE_CURVE('',#8764,#8767,#1642,.T.);
#11008=EDGE_CURVE('',#8768,#8766,#1643,.T.);
#11009=EDGE_CURVE('',#8769,#8768,#1644,.T.);
#11010=EDGE_CURVE('',#8767,#8769,#1645,.T.);
#11011=EDGE_CURVE('',#8770,#8771,#1646,.T.);
#11012=EDGE_CURVE('',#8770,#8772,#7372,.T.);
#11013=EDGE_CURVE('',#8772,#8773,#1647,.T.);
#11014=EDGE_CURVE('',#8771,#8773,#7373,.T.);
#11015=EDGE_CURVE('',#8772,#8769,#1648,.T.);
#11016=EDGE_CURVE('',#8773,#8768,#1649,.T.);
#11017=EDGE_CURVE('',#8774,#8770,#1650,.T.);
#11018=EDGE_CURVE('',#8775,#8774,#1651,.T.);
#11019=EDGE_CURVE('',#8764,#8775,#1652,.T.);
#11020=EDGE_CURVE('',#8776,#8775,#1653,.T.);
#11021=EDGE_CURVE('',#8765,#8776,#1654,.T.);
#11022=EDGE_CURVE('',#8777,#8776,#1655,.T.);
#11023=EDGE_CURVE('',#8771,#8777,#1656,.T.);
#11024=EDGE_CURVE('',#8774,#8777,#1657,.T.);
#11025=EDGE_CURVE('',#8778,#8779,#1658,.T.);
#11026=EDGE_CURVE('',#8778,#8780,#1659,.T.);
#11027=EDGE_CURVE('',#8780,#8781,#1660,.T.);
#11028=EDGE_CURVE('',#8779,#8781,#1661,.T.);
#11029=EDGE_CURVE('',#8782,#8779,#7374,.T.);
#11030=EDGE_CURVE('',#8781,#8783,#1662,.T.);
#11031=EDGE_CURVE('',#8784,#8783,#1663,.T.);
#11032=EDGE_CURVE('',#8784,#8785,#1664,.T.);
#11033=EDGE_CURVE('',#8786,#8785,#1665,.T.);
#11034=EDGE_CURVE('',#8782,#8786,#1666,.T.);
#11035=EDGE_CURVE('',#8787,#8782,#1667,.T.);
#11036=EDGE_CURVE('',#8787,#8778,#7375,.T.);
#11037=EDGE_CURVE('',#8788,#8789,#1668,.T.);
#11038=EDGE_CURVE('',#8789,#8780,#1669,.T.);
#11039=EDGE_CURVE('',#8790,#8787,#1670,.T.);
#11040=EDGE_CURVE('',#8791,#8790,#1671,.T.);
#11041=EDGE_CURVE('',#8788,#8791,#1672,.T.);
#11042=EDGE_CURVE('',#8783,#8789,#1673,.T.);
#11043=EDGE_CURVE('',#8788,#8784,#1674,.T.);
#11044=EDGE_CURVE('',#8785,#8791,#1675,.T.);
#11045=EDGE_CURVE('',#8790,#8786,#1676,.T.);
#11046=EDGE_CURVE('',#8792,#8793,#7376,.T.);
#11047=EDGE_CURVE('',#8794,#8793,#1677,.T.);
#11048=EDGE_CURVE('',#8794,#8795,#7377,.T.);
#11049=EDGE_CURVE('',#8795,#8792,#1678,.T.);
#11050=EDGE_CURVE('',#8793,#8796,#7378,.T.);
#11051=EDGE_CURVE('',#8797,#8796,#1679,.T.);
#11052=EDGE_CURVE('',#8797,#8794,#7379,.T.);
#11053=EDGE_CURVE('',#8796,#8798,#1680,.T.);
#11054=EDGE_CURVE('',#8799,#8798,#1681,.T.);
#11055=EDGE_CURVE('',#8799,#8797,#1682,.T.);
#11056=EDGE_CURVE('',#8798,#8800,#7380,.T.);
#11057=EDGE_CURVE('',#8801,#8800,#1683,.T.);
#11058=EDGE_CURVE('',#8801,#8799,#7381,.T.);
#11059=EDGE_CURVE('',#8800,#8802,#7382,.T.);
#11060=EDGE_CURVE('',#8803,#8802,#1684,.T.);
#11061=EDGE_CURVE('',#8803,#8801,#7383,.T.);
#11062=EDGE_CURVE('',#8802,#8804,#1685,.T.);
#11063=EDGE_CURVE('',#8805,#8804,#1686,.T.);
#11064=EDGE_CURVE('',#8805,#8803,#1687,.T.);
#11065=EDGE_CURVE('',#8804,#8806,#7384,.T.);
#11066=EDGE_CURVE('',#8807,#8806,#1688,.T.);
#11067=EDGE_CURVE('',#8807,#8805,#7385,.T.);
#11068=EDGE_CURVE('',#8806,#8808,#7386,.T.);
#11069=EDGE_CURVE('',#8809,#8808,#1689,.T.);
#11070=EDGE_CURVE('',#8809,#8807,#7387,.T.);
#11071=EDGE_CURVE('',#8808,#8810,#7388,.T.);
#11072=EDGE_CURVE('',#8811,#8810,#1690,.T.);
#11073=EDGE_CURVE('',#8811,#8809,#7389,.T.);
#11074=EDGE_CURVE('',#8810,#8812,#1691,.T.);
#11075=EDGE_CURVE('',#8813,#8812,#1692,.T.);
#11076=EDGE_CURVE('',#8813,#8811,#1693,.T.);
#11077=EDGE_CURVE('',#8812,#8814,#7390,.T.);
#11078=EDGE_CURVE('',#8815,#8814,#1694,.T.);
#11079=EDGE_CURVE('',#8815,#8813,#7391,.T.);
#11080=EDGE_CURVE('',#8814,#8816,#1695,.T.);
#11081=EDGE_CURVE('',#8817,#8816,#1696,.T.);
#11082=EDGE_CURVE('',#8817,#8815,#1697,.T.);
#11083=EDGE_CURVE('',#8816,#8818,#7392,.T.);
#11084=EDGE_CURVE('',#8819,#8818,#1698,.T.);
#11085=EDGE_CURVE('',#8819,#8817,#7393,.T.);
#11086=EDGE_CURVE('',#8818,#8820,#7394,.T.);
#11087=EDGE_CURVE('',#8821,#8820,#1699,.T.);
#11088=EDGE_CURVE('',#8821,#8819,#7395,.T.);
#11089=EDGE_CURVE('',#8820,#8822,#7396,.T.);
#11090=EDGE_CURVE('',#8823,#8822,#1700,.T.);
#11091=EDGE_CURVE('',#8823,#8821,#7397,.T.);
#11092=EDGE_CURVE('',#8822,#8824,#1701,.T.);
#11093=EDGE_CURVE('',#8825,#8824,#1702,.T.);
#11094=EDGE_CURVE('',#8825,#8823,#1703,.T.);
#11095=EDGE_CURVE('',#8824,#8826,#7398,.T.);
#11096=EDGE_CURVE('',#8827,#8826,#1704,.T.);
#11097=EDGE_CURVE('',#8827,#8825,#7399,.T.);
#11098=EDGE_CURVE('',#8826,#8828,#7400,.T.);
#11099=EDGE_CURVE('',#8829,#8828,#1705,.T.);
#11100=EDGE_CURVE('',#8829,#8827,#7401,.T.);
#11101=EDGE_CURVE('',#8828,#8830,#1706,.T.);
#11102=EDGE_CURVE('',#8831,#8830,#1707,.T.);
#11103=EDGE_CURVE('',#8831,#8829,#1708,.T.);
#11104=EDGE_CURVE('',#8830,#8792,#7402,.T.);
#11105=EDGE_CURVE('',#8795,#8831,#7403,.T.);
#11106=EDGE_CURVE('',#8832,#8833,#7404,.T.);
#11107=EDGE_CURVE('',#8833,#8834,#1709,.T.);
#11108=EDGE_CURVE('',#8834,#8835,#7405,.T.);
#11109=EDGE_CURVE('',#8835,#8832,#1710,.T.);
#11110=EDGE_CURVE('',#8836,#8833,#7406,.T.);
#11111=EDGE_CURVE('',#8837,#8836,#1711,.T.);
#11112=EDGE_CURVE('',#8834,#8837,#7407,.T.);
#11113=EDGE_CURVE('',#8836,#8838,#7408,.T.);
#11114=EDGE_CURVE('',#8838,#8839,#1712,.T.);
#11115=EDGE_CURVE('',#8839,#8837,#7409,.T.);
#11116=EDGE_CURVE('',#8840,#8838,#1713,.T.);
#11117=EDGE_CURVE('',#8841,#8840,#1714,.T.);
#11118=EDGE_CURVE('',#8839,#8841,#1715,.T.);
#11119=EDGE_CURVE('',#8842,#8843,#7410,.T.);
#11120=EDGE_CURVE('',#8843,#8844,#1716,.T.);
#11121=EDGE_CURVE('',#8844,#8845,#7411,.T.);
#11122=EDGE_CURVE('',#8845,#8842,#1717,.T.);
#11123=EDGE_CURVE('',#8846,#8843,#7412,.T.);
#11124=EDGE_CURVE('',#8847,#8846,#1718,.T.);
#11125=EDGE_CURVE('',#8844,#8847,#7413,.T.);
#11126=EDGE_CURVE('',#8846,#8848,#7414,.T.);
#11127=EDGE_CURVE('',#8848,#8849,#1719,.T.);
#11128=EDGE_CURVE('',#8849,#8847,#7415,.T.);
#11129=EDGE_CURVE('',#8850,#8848,#1720,.T.);
#11130=EDGE_CURVE('',#8851,#8850,#1721,.T.);
#11131=EDGE_CURVE('',#8849,#8851,#1722,.T.);
#11132=EDGE_CURVE('',#8852,#8853,#7416,.T.);
#11133=EDGE_CURVE('',#8853,#8854,#1723,.T.);
#11134=EDGE_CURVE('',#8854,#8855,#7417,.T.);
#11135=EDGE_CURVE('',#8855,#8852,#1724,.T.);
#11136=EDGE_CURVE('',#8856,#8853,#7418,.T.);
#11137=EDGE_CURVE('',#8857,#8856,#1725,.T.);
#11138=EDGE_CURVE('',#8854,#8857,#7419,.T.);
#11139=EDGE_CURVE('',#8856,#8858,#7420,.T.);
#11140=EDGE_CURVE('',#8858,#8859,#1726,.T.);
#11141=EDGE_CURVE('',#8859,#8857,#7421,.T.);
#11142=EDGE_CURVE('',#8860,#8858,#1727,.T.);
#11143=EDGE_CURVE('',#8861,#8860,#1728,.T.);
#11144=EDGE_CURVE('',#8859,#8861,#1729,.T.);
#11145=EDGE_CURVE('',#8862,#8863,#7422,.T.);
#11146=EDGE_CURVE('',#8863,#8864,#1730,.T.);
#11147=EDGE_CURVE('',#8864,#8865,#7423,.T.);
#11148=EDGE_CURVE('',#8865,#8862,#1731,.T.);
#11149=EDGE_CURVE('',#8866,#8863,#7424,.T.);
#11150=EDGE_CURVE('',#8867,#8866,#1732,.T.);
#11151=EDGE_CURVE('',#8864,#8867,#7425,.T.);
#11152=EDGE_CURVE('',#8866,#8868,#7426,.T.);
#11153=EDGE_CURVE('',#8868,#8869,#1733,.T.);
#11154=EDGE_CURVE('',#8869,#8867,#7427,.T.);
#11155=EDGE_CURVE('',#8870,#8868,#1734,.T.);
#11156=EDGE_CURVE('',#8871,#8870,#1735,.T.);
#11157=EDGE_CURVE('',#8869,#8871,#1736,.T.);
#11158=EDGE_CURVE('',#8872,#8873,#7428,.T.);
#11159=EDGE_CURVE('',#8873,#8874,#1737,.T.);
#11160=EDGE_CURVE('',#8874,#8875,#7429,.T.);
#11161=EDGE_CURVE('',#8875,#8872,#1738,.T.);
#11162=EDGE_CURVE('',#8876,#8873,#7430,.T.);
#11163=EDGE_CURVE('',#8877,#8876,#1739,.T.);
#11164=EDGE_CURVE('',#8874,#8877,#7431,.T.);
#11165=EDGE_CURVE('',#8876,#8878,#7432,.T.);
#11166=EDGE_CURVE('',#8878,#8879,#1740,.T.);
#11167=EDGE_CURVE('',#8879,#8877,#7433,.T.);
#11168=EDGE_CURVE('',#8880,#8878,#1741,.T.);
#11169=EDGE_CURVE('',#8881,#8880,#1742,.T.);
#11170=EDGE_CURVE('',#8879,#8881,#1743,.T.);
#11171=EDGE_CURVE('',#8882,#8875,#1744,.T.);
#11172=EDGE_CURVE('',#8883,#8882,#1745,.T.);
#11173=EDGE_CURVE('',#8872,#8883,#1746,.T.);
#11174=EDGE_CURVE('',#8884,#8865,#1747,.T.);
#11175=EDGE_CURVE('',#8885,#8884,#1748,.T.);
#11176=EDGE_CURVE('',#8862,#8885,#1749,.T.);
#11177=EDGE_CURVE('',#8886,#8845,#1750,.T.);
#11178=EDGE_CURVE('',#8887,#8886,#1751,.T.);
#11179=EDGE_CURVE('',#8842,#8887,#1752,.T.);
#11180=EDGE_CURVE('',#8888,#8835,#1753,.T.);
#11181=EDGE_CURVE('',#8889,#8888,#1754,.T.);
#11182=EDGE_CURVE('',#8832,#8889,#1755,.T.);
#11183=EDGE_CURVE('',#8890,#8880,#7434,.T.);
#11184=EDGE_CURVE('',#8890,#8891,#1756,.T.);
#11185=EDGE_CURVE('',#8881,#8891,#7435,.T.);
#11186=EDGE_CURVE('',#8861,#8884,#7436,.T.);
#11187=EDGE_CURVE('',#8885,#8860,#7437,.T.);
#11188=EDGE_CURVE('',#8891,#8892,#1757,.T.);
#11189=EDGE_CURVE('',#8892,#8893,#7438,.T.);
#11190=EDGE_CURVE('',#8893,#8894,#1758,.T.);
#11191=EDGE_CURVE('',#8894,#8888,#7439,.T.);
#11192=EDGE_CURVE('',#8841,#8886,#7440,.T.);
#11193=EDGE_CURVE('',#8851,#8895,#7441,.T.);
#11194=EDGE_CURVE('',#8895,#8855,#1759,.T.);
#11195=EDGE_CURVE('',#8871,#8882,#7442,.T.);
#11196=EDGE_CURVE('',#8896,#8850,#7443,.T.);
#11197=EDGE_CURVE('',#8896,#8895,#1760,.T.);
#11198=EDGE_CURVE('',#8894,#8897,#1761,.T.);
#11199=EDGE_CURVE('',#8889,#8897,#7444,.T.);
#11200=EDGE_CURVE('',#8852,#8896,#1762,.T.);
#11201=EDGE_CURVE('',#8883,#8870,#7445,.T.);
#11202=EDGE_CURVE('',#8898,#8890,#1763,.T.);
#11203=EDGE_CURVE('',#8892,#8898,#1764,.T.);
#11204=EDGE_CURVE('',#8899,#8898,#7446,.T.);
#11205=EDGE_CURVE('',#8893,#8899,#1765,.T.);
#11206=EDGE_CURVE('',#8897,#8899,#1766,.T.);
#11207=EDGE_CURVE('',#8887,#8840,#7447,.T.);
#11208=EDGE_CURVE('',#8900,#8901,#7448,.T.);
#11209=EDGE_CURVE('',#8902,#8900,#1767,.T.);
#11210=EDGE_CURVE('',#8903,#8902,#324,.T.);
#11211=EDGE_CURVE('',#8901,#8903,#325,.T.);
#11212=EDGE_CURVE('',#8904,#8900,#7449,.T.);
#11213=EDGE_CURVE('',#8905,#8904,#1768,.T.);
#11214=EDGE_CURVE('',#8906,#8905,#326,.T.);
#11215=EDGE_CURVE('',#8907,#8906,#7450,.T.);
#11216=EDGE_CURVE('',#8902,#8907,#327,.T.);
#11217=EDGE_CURVE('',#8908,#8909,#7451,.T.);
#11218=EDGE_CURVE('',#8910,#8908,#1769,.T.);
#11219=EDGE_CURVE('',#8911,#8910,#328,.T.);
#11220=EDGE_CURVE('',#8909,#8911,#329,.T.);
#11221=EDGE_CURVE('',#8912,#8908,#7452,.T.);
#11222=EDGE_CURVE('',#8913,#8912,#1770,.T.);
#11223=EDGE_CURVE('',#8914,#8913,#330,.T.);
#11224=EDGE_CURVE('',#8915,#8914,#7453,.T.);
#11225=EDGE_CURVE('',#8910,#8915,#331,.T.);
#11226=EDGE_CURVE('',#8916,#8917,#7454,.T.);
#11227=EDGE_CURVE('',#8918,#8916,#1771,.T.);
#11228=EDGE_CURVE('',#8919,#8918,#332,.T.);
#11229=EDGE_CURVE('',#8917,#8919,#333,.T.);
#11230=EDGE_CURVE('',#8920,#8916,#7455,.T.);
#11231=EDGE_CURVE('',#8921,#8920,#1772,.T.);
#11232=EDGE_CURVE('',#8922,#8921,#334,.T.);
#11233=EDGE_CURVE('',#8923,#8922,#7456,.T.);
#11234=EDGE_CURVE('',#8918,#8923,#335,.T.);
#11235=EDGE_CURVE('',#8924,#8925,#7457,.T.);
#11236=EDGE_CURVE('',#8926,#8924,#1773,.T.);
#11237=EDGE_CURVE('',#8927,#8926,#336,.T.);
#11238=EDGE_CURVE('',#8925,#8927,#337,.T.);
#11239=EDGE_CURVE('',#8928,#8924,#7458,.T.);
#11240=EDGE_CURVE('',#8929,#8928,#1774,.T.);
#11241=EDGE_CURVE('',#8930,#8929,#338,.T.);
#11242=EDGE_CURVE('',#8931,#8930,#7459,.T.);
#11243=EDGE_CURVE('',#8926,#8931,#339,.T.);
#11244=EDGE_CURVE('',#8932,#8904,#7460,.T.);
#11245=EDGE_CURVE('',#8933,#8932,#340,.T.);
#11246=EDGE_CURVE('',#8905,#8933,#341,.T.);
#11247=EDGE_CURVE('',#8934,#8912,#7461,.T.);
#11248=EDGE_CURVE('',#8935,#8934,#342,.T.);
#11249=EDGE_CURVE('',#8913,#8935,#343,.T.);
#11250=EDGE_CURVE('',#8936,#8920,#7462,.T.);
#11251=EDGE_CURVE('',#8937,#8936,#344,.T.);
#11252=EDGE_CURVE('',#8921,#8937,#345,.T.);
#11253=EDGE_CURVE('',#8938,#8928,#7463,.T.);
#11254=EDGE_CURVE('',#8939,#8938,#346,.T.);
#11255=EDGE_CURVE('',#8929,#8939,#347,.T.);
#11256=EDGE_CURVE('',#8935,#8903,#1775,.T.);
#11257=EDGE_CURVE('',#8934,#8901,#1776,.T.);
#11258=EDGE_CURVE('',#8907,#8914,#1777,.T.);
#11259=EDGE_CURVE('',#8937,#8911,#1778,.T.);
#11260=EDGE_CURVE('',#8936,#8909,#1779,.T.);
#11261=EDGE_CURVE('',#8915,#8922,#1780,.T.);
#11262=EDGE_CURVE('',#8939,#8919,#1781,.T.);
#11263=EDGE_CURVE('',#8938,#8917,#1782,.T.);
#11264=EDGE_CURVE('',#8932,#8925,#1783,.T.);
#11265=EDGE_CURVE('',#8940,#8941,#1784,.T.);
#11266=EDGE_CURVE('',#8941,#8942,#1785,.T.);
#11267=EDGE_CURVE('',#8942,#8943,#1786,.T.);
#11268=EDGE_CURVE('',#8943,#8944,#1787,.T.);
#11269=EDGE_CURVE('',#8944,#8945,#1788,.T.);
#11270=EDGE_CURVE('',#8945,#8946,#1789,.T.);
#11271=EDGE_CURVE('',#8946,#8947,#1790,.T.);
#11272=EDGE_CURVE('',#8947,#8940,#1791,.T.);
#11273=EDGE_CURVE('',#8948,#8948,#7464,.T.);
#11274=EDGE_CURVE('',#8949,#8949,#7465,.T.);
#11275=EDGE_CURVE('',#8950,#8950,#7466,.T.);
#11276=EDGE_CURVE('',#8951,#8951,#7467,.T.);
#11277=EDGE_CURVE('',#8923,#8930,#1792,.T.);
#11278=EDGE_CURVE('',#8931,#8906,#1793,.T.);
#11279=EDGE_CURVE('',#8952,#8952,#7468,.T.);
#11280=EDGE_CURVE('',#8953,#8953,#7469,.T.);
#11281=EDGE_CURVE('',#8954,#8954,#7470,.T.);
#11282=EDGE_CURVE('',#8955,#8955,#7471,.T.);
#11283=EDGE_CURVE('',#8956,#8956,#7472,.T.);
#11284=EDGE_CURVE('',#8957,#8958,#1794,.T.);
#11285=EDGE_CURVE('',#8958,#8959,#1795,.T.);
#11286=EDGE_CURVE('',#8959,#8960,#1796,.T.);
#11287=EDGE_CURVE('',#8957,#8960,#1797,.T.);
#11288=EDGE_CURVE('',#8958,#8961,#1798,.T.);
#11289=EDGE_CURVE('',#8961,#8962,#1799,.T.);
#11290=EDGE_CURVE('',#8962,#8959,#1800,.T.);
#11291=EDGE_CURVE('',#8961,#8963,#1801,.T.);
#11292=EDGE_CURVE('',#8963,#8964,#1802,.T.);
#11293=EDGE_CURVE('',#8964,#8962,#1803,.T.);
#11294=EDGE_CURVE('',#8965,#8964,#1804,.T.);
#11295=EDGE_CURVE('',#8963,#8966,#1805,.T.);
#11296=EDGE_CURVE('',#8966,#8965,#1806,.T.);
#11297=EDGE_CURVE('',#8967,#8965,#1807,.T.);
#11298=EDGE_CURVE('',#8966,#8968,#1808,.T.);
#11299=EDGE_CURVE('',#8968,#8967,#1809,.T.);
#11300=EDGE_CURVE('',#8969,#8967,#1810,.T.);
#11301=EDGE_CURVE('',#8968,#8970,#1811,.T.);
#11302=EDGE_CURVE('',#8970,#8969,#1812,.T.);
#11303=EDGE_CURVE('',#8971,#8969,#1813,.T.);
#11304=EDGE_CURVE('',#8970,#8972,#1814,.T.);
#11305=EDGE_CURVE('',#8972,#8971,#1815,.T.);
#11306=EDGE_CURVE('',#8960,#8971,#1816,.T.);
#11307=EDGE_CURVE('',#8972,#8957,#1817,.T.);
#11308=EDGE_CURVE('',#8947,#8969,#1818,.T.);
#11309=EDGE_CURVE('',#8946,#8967,#1819,.T.);
#11310=EDGE_CURVE('',#8940,#8971,#1820,.T.);
#11311=EDGE_CURVE('',#8941,#8960,#1821,.T.);
#11312=EDGE_CURVE('',#8942,#8959,#1822,.T.);
#11313=EDGE_CURVE('',#8973,#8973,#7473,.T.);
#11314=EDGE_CURVE('',#8933,#8927,#1823,.T.);
#11315=EDGE_CURVE('',#8974,#8975,#7474,.T.);
#11316=EDGE_CURVE('',#8975,#8976,#1824,.T.);
#11317=EDGE_CURVE('',#8976,#8976,#7475,.T.);
#11318=EDGE_CURVE('',#8975,#8974,#7476,.T.);
#11319=EDGE_CURVE('',#8977,#8977,#7477,.T.);
#11320=EDGE_CURVE('',#8974,#8956,#1825,.T.);
#11321=EDGE_CURVE('',#8978,#8979,#7478,.T.);
#11322=EDGE_CURVE('',#8979,#8977,#1826,.T.);
#11323=EDGE_CURVE('',#8979,#8978,#7479,.T.);
#11324=EDGE_CURVE('',#8980,#8980,#7480,.T.);
#11325=EDGE_CURVE('',#8980,#8978,#1827,.T.);
#11326=EDGE_CURVE('',#8980,#8981,#1828,.T.);
#11327=EDGE_CURVE('',#8981,#8981,#7481,.T.);
#11328=EDGE_CURVE('',#8982,#8982,#7482,.T.);
#11329=EDGE_CURVE('',#8983,#8983,#7483,.T.);
#11330=EDGE_CURVE('',#8983,#8984,#1829,.T.);
#11331=EDGE_CURVE('',#8984,#8984,#7484,.T.);
#11332=EDGE_CURVE('',#8985,#8985,#7485,.T.);
#11333=EDGE_CURVE('',#8973,#8983,#1830,.T.);
#11334=EDGE_CURVE('',#8986,#8987,#7486,.T.);
#11335=EDGE_CURVE('',#8987,#8985,#1831,.T.);
#11336=EDGE_CURVE('',#8987,#8986,#7487,.T.);
#11337=EDGE_CURVE('',#8986,#8988,#1832,.T.);
#11338=EDGE_CURVE('',#8988,#8988,#7488,.T.);
#11339=EDGE_CURVE('',#8951,#8952,#1833,.T.);
#11340=EDGE_CURVE('',#8950,#8953,#1834,.T.);
#11341=EDGE_CURVE('',#8949,#8954,#1835,.T.);
#11342=EDGE_CURVE('',#8948,#8955,#1836,.T.);
#11343=EDGE_CURVE('',#8989,#8989,#7489,.T.);
#11344=EDGE_CURVE('',#8989,#8982,#1837,.T.);
#11345=EDGE_CURVE('',#8945,#8965,#1838,.T.);
#11346=EDGE_CURVE('',#8944,#8964,#1839,.T.);
#11347=EDGE_CURVE('',#8943,#8962,#1840,.T.);
#11348=EDGE_CURVE('',#8990,#8991,#7490,.T.);
#11349=EDGE_CURVE('',#8991,#8992,#1841,.T.);
#11350=EDGE_CURVE('',#8992,#8993,#7491,.T.);
#11351=EDGE_CURVE('',#8993,#8990,#1842,.T.);
#11352=EDGE_CURVE('',#8994,#8991,#7492,.T.);
#11353=EDGE_CURVE('',#8995,#8994,#1843,.T.);
#11354=EDGE_CURVE('',#8992,#8995,#7493,.T.);
#11355=EDGE_CURVE('',#8994,#8996,#7494,.T.);
#11356=EDGE_CURVE('',#8996,#8997,#1844,.T.);
#11357=EDGE_CURVE('',#8997,#8995,#7495,.T.);
#11358=EDGE_CURVE('',#8998,#8996,#1845,.T.);
#11359=EDGE_CURVE('',#8999,#8998,#1846,.T.);
#11360=EDGE_CURVE('',#8997,#8999,#1847,.T.);
#11361=EDGE_CURVE('',#9000,#9001,#7496,.T.);
#11362=EDGE_CURVE('',#9001,#9002,#1848,.T.);
#11363=EDGE_CURVE('',#9002,#9003,#7497,.T.);
#11364=EDGE_CURVE('',#9003,#9000,#1849,.T.);
#11365=EDGE_CURVE('',#9004,#9001,#7498,.T.);
#11366=EDGE_CURVE('',#9005,#9004,#1850,.T.);
#11367=EDGE_CURVE('',#9002,#9005,#7499,.T.);
#11368=EDGE_CURVE('',#9004,#9006,#7500,.T.);
#11369=EDGE_CURVE('',#9006,#9007,#1851,.T.);
#11370=EDGE_CURVE('',#9007,#9005,#7501,.T.);
#11371=EDGE_CURVE('',#9008,#9006,#1852,.T.);
#11372=EDGE_CURVE('',#9009,#9008,#1853,.T.);
#11373=EDGE_CURVE('',#9007,#9009,#1854,.T.);
#11374=EDGE_CURVE('',#9010,#9011,#7502,.T.);
#11375=EDGE_CURVE('',#9011,#9012,#1855,.T.);
#11376=EDGE_CURVE('',#9012,#9013,#7503,.T.);
#11377=EDGE_CURVE('',#9013,#9010,#1856,.T.);
#11378=EDGE_CURVE('',#9014,#9011,#7504,.T.);
#11379=EDGE_CURVE('',#9015,#9014,#1857,.T.);
#11380=EDGE_CURVE('',#9012,#9015,#7505,.T.);
#11381=EDGE_CURVE('',#9014,#9016,#7506,.T.);
#11382=EDGE_CURVE('',#9016,#9017,#1858,.T.);
#11383=EDGE_CURVE('',#9017,#9015,#7507,.T.);
#11384=EDGE_CURVE('',#9018,#9016,#1859,.T.);
#11385=EDGE_CURVE('',#9019,#9018,#1860,.T.);
#11386=EDGE_CURVE('',#9017,#9019,#1861,.T.);
#11387=EDGE_CURVE('',#9020,#9021,#7508,.T.);
#11388=EDGE_CURVE('',#9021,#9022,#1862,.T.);
#11389=EDGE_CURVE('',#9022,#9023,#7509,.T.);
#11390=EDGE_CURVE('',#9023,#9020,#1863,.T.);
#11391=EDGE_CURVE('',#9024,#9021,#7510,.T.);
#11392=EDGE_CURVE('',#9025,#9024,#1864,.T.);
#11393=EDGE_CURVE('',#9022,#9025,#7511,.T.);
#11394=EDGE_CURVE('',#9024,#9026,#7512,.T.);
#11395=EDGE_CURVE('',#9026,#9027,#1865,.T.);
#11396=EDGE_CURVE('',#9027,#9025,#7513,.T.);
#11397=EDGE_CURVE('',#9028,#9026,#1866,.T.);
#11398=EDGE_CURVE('',#9029,#9028,#1867,.T.);
#11399=EDGE_CURVE('',#9027,#9029,#1868,.T.);
#11400=EDGE_CURVE('',#9030,#9031,#7514,.T.);
#11401=EDGE_CURVE('',#9031,#9032,#1869,.T.);
#11402=EDGE_CURVE('',#9032,#9033,#7515,.T.);
#11403=EDGE_CURVE('',#9033,#9030,#1870,.T.);
#11404=EDGE_CURVE('',#9034,#9031,#7516,.T.);
#11405=EDGE_CURVE('',#9035,#9034,#1871,.T.);
#11406=EDGE_CURVE('',#9032,#9035,#7517,.T.);
#11407=EDGE_CURVE('',#9034,#9036,#7518,.T.);
#11408=EDGE_CURVE('',#9036,#9037,#1872,.T.);
#11409=EDGE_CURVE('',#9037,#9035,#7519,.T.);
#11410=EDGE_CURVE('',#9038,#9036,#1873,.T.);
#11411=EDGE_CURVE('',#9039,#9038,#1874,.T.);
#11412=EDGE_CURVE('',#9037,#9039,#1875,.T.);
#11413=EDGE_CURVE('',#9040,#9033,#1876,.T.);
#11414=EDGE_CURVE('',#9041,#9040,#1877,.T.);
#11415=EDGE_CURVE('',#9030,#9041,#1878,.T.);
#11416=EDGE_CURVE('',#9042,#9023,#1879,.T.);
#11417=EDGE_CURVE('',#9043,#9042,#1880,.T.);
#11418=EDGE_CURVE('',#9020,#9043,#1881,.T.);
#11419=EDGE_CURVE('',#9044,#9003,#1882,.T.);
#11420=EDGE_CURVE('',#9045,#9044,#1883,.T.);
#11421=EDGE_CURVE('',#9000,#9045,#1884,.T.);
#11422=EDGE_CURVE('',#9046,#8993,#1885,.T.);
#11423=EDGE_CURVE('',#9047,#9046,#1886,.T.);
#11424=EDGE_CURVE('',#8990,#9047,#1887,.T.);
#11425=EDGE_CURVE('',#9048,#9038,#7520,.T.);
#11426=EDGE_CURVE('',#9048,#9049,#1888,.T.);
#11427=EDGE_CURVE('',#9039,#9049,#7521,.T.);
#11428=EDGE_CURVE('',#9019,#9042,#7522,.T.);
#11429=EDGE_CURVE('',#9043,#9018,#7523,.T.);
#11430=EDGE_CURVE('',#9049,#9050,#1889,.T.);
#11431=EDGE_CURVE('',#9050,#9051,#7524,.T.);
#11432=EDGE_CURVE('',#9051,#9052,#1890,.T.);
#11433=EDGE_CURVE('',#9052,#9046,#7525,.T.);
#11434=EDGE_CURVE('',#8999,#9044,#7526,.T.);
#11435=EDGE_CURVE('',#9009,#9053,#7527,.T.);
#11436=EDGE_CURVE('',#9053,#9013,#1891,.T.);
#11437=EDGE_CURVE('',#9029,#9040,#7528,.T.);
#11438=EDGE_CURVE('',#9054,#9008,#7529,.T.);
#11439=EDGE_CURVE('',#9054,#9053,#1892,.T.);
#11440=EDGE_CURVE('',#9052,#9055,#1893,.T.);
#11441=EDGE_CURVE('',#9047,#9055,#7530,.T.);
#11442=EDGE_CURVE('',#9010,#9054,#1894,.T.);
#11443=EDGE_CURVE('',#9041,#9028,#7531,.T.);
#11444=EDGE_CURVE('',#9056,#9048,#1895,.T.);
#11445=EDGE_CURVE('',#9050,#9056,#1896,.T.);
#11446=EDGE_CURVE('',#9057,#9056,#7532,.T.);
#11447=EDGE_CURVE('',#9051,#9057,#1897,.T.);
#11448=EDGE_CURVE('',#9055,#9057,#1898,.T.);
#11449=EDGE_CURVE('',#9045,#8998,#7533,.T.);
#11450=EDGE_CURVE('',#9058,#9059,#1899,.T.);
#11451=EDGE_CURVE('',#9058,#9060,#7534,.T.);
#11452=EDGE_CURVE('',#9060,#9061,#7535,.T.);
#11453=EDGE_CURVE('',#9061,#9062,#156,.T.);
#11454=EDGE_CURVE('',#9062,#9059,#7536,.T.);
#11455=EDGE_CURVE('',#9059,#9062,#7537,.T.);
#11456=EDGE_CURVE('',#9062,#9063,#157,.T.);
#11457=EDGE_CURVE('',#9063,#9058,#7538,.T.);
#11458=EDGE_CURVE('',#9064,#9064,#7539,.T.);
#11459=EDGE_CURVE('',#9064,#9065,#1900,.T.);
#11460=EDGE_CURVE('',#9065,#9065,#7540,.T.);
#11461=EDGE_CURVE('',#9066,#9066,#7541,.T.);
#11462=EDGE_CURVE('',#9067,#9067,#7542,.T.);
#11463=EDGE_CURVE('',#9068,#9061,#1901,.T.);
#11464=EDGE_CURVE('',#9060,#9067,#1902,.T.);
#11465=EDGE_CURVE('',#9063,#9069,#1903,.T.);
#11466=EDGE_CURVE('',#9069,#9068,#7543,.T.);
#11467=EDGE_CURVE('',#9068,#9069,#1904,.T.);
#11468=EDGE_CURVE('',#9066,#9070,#1905,.T.);
#11469=EDGE_CURVE('',#9071,#9070,#7544,.T.);
#11470=EDGE_CURVE('',#9070,#9071,#7545,.T.);
#11471=EDGE_CURVE('',#9071,#9072,#1906,.T.);
#11472=EDGE_CURVE('',#9072,#9072,#7546,.T.);
#11473=EDGE_CURVE('',#9073,#9074,#1907,.T.);
#11474=EDGE_CURVE('',#9073,#9075,#1908,.T.);
#11475=EDGE_CURVE('',#9076,#9075,#1909,.T.);
#11476=EDGE_CURVE('',#9074,#9076,#1910,.T.);
#11477=EDGE_CURVE('',#9077,#9078,#1911,.T.);
#11478=EDGE_CURVE('',#9077,#9079,#1912,.T.);
#11479=EDGE_CURVE('',#9080,#9079,#1913,.T.);
#11480=EDGE_CURVE('',#9078,#9080,#1914,.T.);
#11481=EDGE_CURVE('',#9081,#9073,#1915,.T.);
#11482=EDGE_CURVE('',#9082,#9081,#1916,.T.);
#11483=EDGE_CURVE('',#9075,#9082,#1917,.T.);
#11484=EDGE_CURVE('',#9083,#9077,#1918,.T.);
#11485=EDGE_CURVE('',#9084,#9083,#1919,.T.);
#11486=EDGE_CURVE('',#9079,#9084,#1920,.T.);
#11487=EDGE_CURVE('',#9076,#9085,#1921,.T.);
#11488=EDGE_CURVE('',#9085,#9086,#1922,.T.);
#11489=EDGE_CURVE('',#9074,#9086,#1923,.T.);
#11490=EDGE_CURVE('',#9082,#9083,#1924,.T.);
#11491=EDGE_CURVE('',#9078,#9087,#1925,.T.);
#11492=EDGE_CURVE('',#9087,#9088,#1926,.T.);
#11493=EDGE_CURVE('',#9088,#9089,#1927,.T.);
#11494=EDGE_CURVE('',#9089,#9090,#1928,.T.);
#11495=EDGE_CURVE('',#9091,#9090,#7547,.T.);
#11496=EDGE_CURVE('',#9092,#9091,#1929,.T.);
#11497=EDGE_CURVE('',#9093,#9092,#1930,.T.);
#11498=EDGE_CURVE('',#9085,#9093,#1931,.T.);
#11499=EDGE_CURVE('',#9080,#9094,#1932,.T.);
#11500=EDGE_CURVE('',#9087,#9094,#1933,.T.);
#11501=EDGE_CURVE('',#9089,#9095,#1934,.T.);
#11502=EDGE_CURVE('',#9095,#9096,#1935,.T.);
#11503=EDGE_CURVE('',#9090,#9096,#1936,.T.);
#11504=EDGE_CURVE('',#9088,#9097,#1937,.T.);
#11505=EDGE_CURVE('',#9097,#9095,#1938,.T.);
#11506=EDGE_CURVE('',#9094,#9097,#1939,.T.);
#11507=EDGE_CURVE('',#9081,#9084,#1940,.T.);
#11508=EDGE_CURVE('',#9098,#9096,#7548,.T.);
#11509=EDGE_CURVE('',#9091,#9098,#1941,.T.);
#11510=EDGE_CURVE('',#9099,#9098,#1942,.T.);
#11511=EDGE_CURVE('',#9092,#9099,#1943,.T.);
#11512=EDGE_CURVE('',#9100,#9099,#1944,.T.);
#11513=EDGE_CURVE('',#9093,#9100,#1945,.T.);
#11514=EDGE_CURVE('',#9086,#9100,#1946,.T.);
#11515=EDGE_CURVE('',#9101,#9101,#7549,.T.);
#11516=EDGE_CURVE('',#9101,#9102,#1947,.T.);
#11517=EDGE_CURVE('',#9102,#9102,#7550,.T.);
#11518=EDGE_CURVE('',#9103,#9103,#7551,.T.);
#11519=EDGE_CURVE('',#9103,#9104,#1948,.T.);
#11520=EDGE_CURVE('',#9104,#9104,#7552,.T.);
#11521=EDGE_CURVE('',#9105,#9105,#7553,.T.);
#11522=EDGE_CURVE('',#9105,#9106,#1949,.T.);
#11523=EDGE_CURVE('',#9106,#9106,#7554,.T.);
#11524=EDGE_CURVE('',#9107,#9107,#7555,.T.);
#11525=EDGE_CURVE('',#9107,#9108,#1950,.T.);
#11526=EDGE_CURVE('',#9108,#9108,#7556,.T.);
#11527=EDGE_CURVE('',#9109,#9109,#7557,.T.);
#11528=EDGE_CURVE('',#9109,#9110,#1951,.T.);
#11529=EDGE_CURVE('',#9110,#9110,#7558,.T.);
#11530=EDGE_CURVE('',#9111,#9111,#7559,.T.);
#11531=EDGE_CURVE('',#9111,#9112,#1952,.T.);
#11532=EDGE_CURVE('',#9112,#9112,#7560,.T.);
#11533=EDGE_CURVE('',#9113,#9113,#7561,.T.);
#11534=EDGE_CURVE('',#9113,#9114,#1953,.T.);
#11535=EDGE_CURVE('',#9114,#9114,#7562,.T.);
#11536=EDGE_CURVE('',#9115,#9115,#7563,.T.);
#11537=EDGE_CURVE('',#9115,#9116,#1954,.T.);
#11538=EDGE_CURVE('',#9116,#9116,#7564,.T.);
#11539=EDGE_CURVE('',#9117,#9117,#7565,.T.);
#11540=EDGE_CURVE('',#9117,#9118,#1955,.T.);
#11541=EDGE_CURVE('',#9118,#9118,#7566,.T.);
#11542=EDGE_CURVE('',#9119,#9119,#7567,.T.);
#11543=EDGE_CURVE('',#9119,#9120,#1956,.T.);
#11544=EDGE_CURVE('',#9120,#9120,#7568,.T.);
#11545=EDGE_CURVE('',#9121,#9122,#1957,.T.);
#11546=EDGE_CURVE('',#9121,#9123,#1958,.T.);
#11547=EDGE_CURVE('',#9123,#9124,#1959,.T.);
#11548=EDGE_CURVE('',#9122,#9124,#1960,.T.);
#11549=EDGE_CURVE('',#9125,#9121,#1961,.T.);
#11550=EDGE_CURVE('',#9125,#9126,#1962,.T.);
#11551=EDGE_CURVE('',#9126,#9123,#1963,.T.);
#11552=EDGE_CURVE('',#9127,#9128,#1964,.T.);
#11553=EDGE_CURVE('',#9127,#9129,#1965,.T.);
#11554=EDGE_CURVE('',#9129,#9130,#1966,.T.);
#11555=EDGE_CURVE('',#9128,#9130,#1967,.T.);
#11556=EDGE_CURVE('',#9122,#9127,#1968,.T.);
#11557=EDGE_CURVE('',#9124,#9129,#1969,.T.);
#11558=EDGE_CURVE('',#9131,#9132,#1970,.T.);
#11559=EDGE_CURVE('',#9132,#9133,#1971,.T.);
#11560=EDGE_CURVE('',#9134,#9133,#1972,.T.);
#11561=EDGE_CURVE('',#9131,#9134,#1973,.T.);
#11562=EDGE_CURVE('',#9135,#9131,#1974,.T.);
#11563=EDGE_CURVE('',#9136,#9134,#1975,.T.);
#11564=EDGE_CURVE('',#9135,#9136,#1976,.T.);
#11565=EDGE_CURVE('',#9135,#9125,#1977,.T.);
#11566=EDGE_CURVE('',#9136,#9126,#1978,.T.);
#11567=EDGE_CURVE('',#9137,#9128,#7569,.T.);
#11568=EDGE_CURVE('',#9138,#9130,#7570,.T.);
#11569=EDGE_CURVE('',#9137,#9138,#1979,.T.);
#11570=EDGE_CURVE('',#9139,#9137,#1980,.T.);
#11571=EDGE_CURVE('',#9140,#9138,#1981,.T.);
#11572=EDGE_CURVE('',#9139,#9140,#1982,.T.);
#11573=EDGE_CURVE('',#9132,#9139,#1983,.T.);
#11574=EDGE_CURVE('',#9133,#9140,#1984,.T.);
#11575=EDGE_CURVE('',#9141,#9142,#1985,.T.);
#11576=EDGE_CURVE('',#9142,#9143,#1986,.T.);
#11577=EDGE_CURVE('',#9143,#9144,#1987,.T.);
#11578=EDGE_CURVE('',#9141,#9144,#1988,.T.);
#11579=EDGE_CURVE('',#9145,#9143,#1989,.T.);
#11580=EDGE_CURVE('',#9146,#9145,#1990,.T.);
#11581=EDGE_CURVE('',#9144,#9146,#1991,.T.);
#11582=EDGE_CURVE('',#9147,#9148,#1992,.T.);
#11583=EDGE_CURVE('',#9147,#9149,#7571,.T.);
#11584=EDGE_CURVE('',#9149,#9150,#1993,.T.);
#11585=EDGE_CURVE('',#9148,#9150,#7572,.T.);
#11586=EDGE_CURVE('',#9149,#9146,#1994,.T.);
#11587=EDGE_CURVE('',#9150,#9145,#1995,.T.);
#11588=EDGE_CURVE('',#9151,#9148,#1996,.T.);
#11589=EDGE_CURVE('',#9152,#9151,#1997,.T.);
#11590=EDGE_CURVE('',#9147,#9152,#1998,.T.);
#11591=EDGE_CURVE('',#9153,#9152,#1999,.T.);
#11592=EDGE_CURVE('',#9141,#9153,#2000,.T.);
#11593=EDGE_CURVE('',#9154,#9153,#2001,.T.);
#11594=EDGE_CURVE('',#9142,#9154,#2002,.T.);
#11595=EDGE_CURVE('',#9151,#9154,#2003,.T.);
#11596=EDGE_CURVE('',#9155,#9156,#7573,.T.);
#11597=EDGE_CURVE('',#9156,#9157,#2004,.T.);
#11598=EDGE_CURVE('',#9157,#9158,#7574,.T.);
#11599=EDGE_CURVE('',#9158,#9155,#2005,.T.);
#11600=EDGE_CURVE('',#9159,#9156,#7575,.T.);
#11601=EDGE_CURVE('',#9160,#9159,#2006,.T.);
#11602=EDGE_CURVE('',#9157,#9160,#7576,.T.);
#11603=EDGE_CURVE('',#9159,#9161,#7577,.T.);
#11604=EDGE_CURVE('',#9161,#9162,#2007,.T.);
#11605=EDGE_CURVE('',#9162,#9160,#7578,.T.);
#11606=EDGE_CURVE('',#9163,#9161,#2008,.T.);
#11607=EDGE_CURVE('',#9164,#9163,#2009,.T.);
#11608=EDGE_CURVE('',#9162,#9164,#2010,.T.);
#11609=EDGE_CURVE('',#9165,#9166,#7579,.T.);
#11610=EDGE_CURVE('',#9166,#9167,#2011,.T.);
#11611=EDGE_CURVE('',#9167,#9168,#7580,.T.);
#11612=EDGE_CURVE('',#9168,#9165,#2012,.T.);
#11613=EDGE_CURVE('',#9169,#9166,#7581,.T.);
#11614=EDGE_CURVE('',#9170,#9169,#2013,.T.);
#11615=EDGE_CURVE('',#9167,#9170,#7582,.T.);
#11616=EDGE_CURVE('',#9169,#9171,#7583,.T.);
#11617=EDGE_CURVE('',#9171,#9172,#2014,.T.);
#11618=EDGE_CURVE('',#9172,#9170,#7584,.T.);
#11619=EDGE_CURVE('',#9173,#9171,#2015,.T.);
#11620=EDGE_CURVE('',#9174,#9173,#2016,.T.);
#11621=EDGE_CURVE('',#9172,#9174,#2017,.T.);
#11622=EDGE_CURVE('',#9175,#9176,#7585,.T.);
#11623=EDGE_CURVE('',#9176,#9177,#2018,.T.);
#11624=EDGE_CURVE('',#9177,#9178,#7586,.T.);
#11625=EDGE_CURVE('',#9178,#9175,#2019,.T.);
#11626=EDGE_CURVE('',#9179,#9176,#7587,.T.);
#11627=EDGE_CURVE('',#9180,#9179,#2020,.T.);
#11628=EDGE_CURVE('',#9177,#9180,#7588,.T.);
#11629=EDGE_CURVE('',#9179,#9181,#7589,.T.);
#11630=EDGE_CURVE('',#9181,#9182,#2021,.T.);
#11631=EDGE_CURVE('',#9182,#9180,#7590,.T.);
#11632=EDGE_CURVE('',#9183,#9181,#2022,.T.);
#11633=EDGE_CURVE('',#9184,#9183,#2023,.T.);
#11634=EDGE_CURVE('',#9182,#9184,#2024,.T.);
#11635=EDGE_CURVE('',#9185,#9186,#7591,.T.);
#11636=EDGE_CURVE('',#9186,#9187,#2025,.T.);
#11637=EDGE_CURVE('',#9187,#9188,#7592,.T.);
#11638=EDGE_CURVE('',#9188,#9185,#2026,.T.);
#11639=EDGE_CURVE('',#9189,#9186,#7593,.T.);
#11640=EDGE_CURVE('',#9190,#9189,#2027,.T.);
#11641=EDGE_CURVE('',#9187,#9190,#7594,.T.);
#11642=EDGE_CURVE('',#9189,#9191,#7595,.T.);
#11643=EDGE_CURVE('',#9191,#9192,#2028,.T.);
#11644=EDGE_CURVE('',#9192,#9190,#7596,.T.);
#11645=EDGE_CURVE('',#9193,#9191,#2029,.T.);
#11646=EDGE_CURVE('',#9194,#9193,#2030,.T.);
#11647=EDGE_CURVE('',#9192,#9194,#2031,.T.);
#11648=EDGE_CURVE('',#9195,#9196,#7597,.T.);
#11649=EDGE_CURVE('',#9196,#9197,#2032,.T.);
#11650=EDGE_CURVE('',#9197,#9198,#7598,.T.);
#11651=EDGE_CURVE('',#9198,#9195,#2033,.T.);
#11652=EDGE_CURVE('',#9199,#9196,#7599,.T.);
#11653=EDGE_CURVE('',#9200,#9199,#2034,.T.);
#11654=EDGE_CURVE('',#9197,#9200,#7600,.T.);
#11655=EDGE_CURVE('',#9199,#9201,#7601,.T.);
#11656=EDGE_CURVE('',#9201,#9202,#2035,.T.);
#11657=EDGE_CURVE('',#9202,#9200,#7602,.T.);
#11658=EDGE_CURVE('',#9203,#9201,#2036,.T.);
#11659=EDGE_CURVE('',#9204,#9203,#2037,.T.);
#11660=EDGE_CURVE('',#9202,#9204,#2038,.T.);
#11661=EDGE_CURVE('',#9205,#9198,#2039,.T.);
#11662=EDGE_CURVE('',#9206,#9205,#2040,.T.);
#11663=EDGE_CURVE('',#9195,#9206,#2041,.T.);
#11664=EDGE_CURVE('',#9207,#9188,#2042,.T.);
#11665=EDGE_CURVE('',#9208,#9207,#2043,.T.);
#11666=EDGE_CURVE('',#9185,#9208,#2044,.T.);
#11667=EDGE_CURVE('',#9209,#9168,#2045,.T.);
#11668=EDGE_CURVE('',#9210,#9209,#2046,.T.);
#11669=EDGE_CURVE('',#9165,#9210,#2047,.T.);
#11670=EDGE_CURVE('',#9211,#9158,#2048,.T.);
#11671=EDGE_CURVE('',#9212,#9211,#2049,.T.);
#11672=EDGE_CURVE('',#9155,#9212,#2050,.T.);
#11673=EDGE_CURVE('',#9213,#9203,#7603,.T.);
#11674=EDGE_CURVE('',#9214,#9213,#2051,.T.);
#11675=EDGE_CURVE('',#9204,#9214,#7604,.T.);
#11676=EDGE_CURVE('',#9184,#9207,#7605,.T.);
#11677=EDGE_CURVE('',#9208,#9183,#7606,.T.);
#11678=EDGE_CURVE('',#9214,#9215,#2052,.T.);
#11679=EDGE_CURVE('',#9215,#9216,#7607,.T.);
#11680=EDGE_CURVE('',#9216,#9217,#2053,.T.);
#11681=EDGE_CURVE('',#9217,#9211,#7608,.T.);
#11682=EDGE_CURVE('',#9164,#9209,#7609,.T.);
#11683=EDGE_CURVE('',#9174,#9218,#7610,.T.);
#11684=EDGE_CURVE('',#9218,#9178,#2054,.T.);
#11685=EDGE_CURVE('',#9194,#9205,#7611,.T.);
#11686=EDGE_CURVE('',#9219,#9173,#7612,.T.);
#11687=EDGE_CURVE('',#9219,#9218,#2055,.T.);
#11688=EDGE_CURVE('',#9217,#9220,#2056,.T.);
#11689=EDGE_CURVE('',#9212,#9220,#7613,.T.);
#11690=EDGE_CURVE('',#9175,#9219,#2057,.T.);
#11691=EDGE_CURVE('',#9206,#9193,#7614,.T.);
#11692=EDGE_CURVE('',#9221,#9215,#2058,.T.);
#11693=EDGE_CURVE('',#9222,#9221,#7615,.T.);
#11694=EDGE_CURVE('',#9216,#9222,#2059,.T.);
#11695=EDGE_CURVE('',#9220,#9222,#2060,.T.);
#11696=EDGE_CURVE('',#9210,#9163,#7616,.T.);
#11697=EDGE_CURVE('',#9221,#9213,#2061,.T.);
#11698=EDGE_CURVE('',#9223,#9223,#7617,.T.);
#11699=EDGE_CURVE('',#9224,#9224,#7618,.T.);
#11700=EDGE_CURVE('',#9224,#9225,#2062,.T.);
#11701=EDGE_CURVE('',#9225,#9225,#7619,.T.);
#11702=EDGE_CURVE('',#9226,#9226,#7620,.T.);
#11703=EDGE_CURVE('',#9226,#9223,#2063,.T.);
#11704=EDGE_CURVE('',#9227,#9228,#2064,.T.);
#11705=EDGE_CURVE('',#9228,#9229,#2065,.T.);
#11706=EDGE_CURVE('',#9229,#9230,#2066,.T.);
#11707=EDGE_CURVE('',#9227,#9230,#2067,.T.);
#11708=EDGE_CURVE('',#9231,#9229,#2068,.T.);
#11709=EDGE_CURVE('',#9232,#9231,#2069,.T.);
#11710=EDGE_CURVE('',#9230,#9232,#2070,.T.);
#11711=EDGE_CURVE('',#9233,#9232,#2071,.T.);
#11712=EDGE_CURVE('',#9234,#9233,#7621,.T.);
#11713=EDGE_CURVE('',#9234,#9235,#2072,.T.);
#11714=EDGE_CURVE('',#9236,#9235,#2073,.T.);
#11715=EDGE_CURVE('',#9236,#9227,#2074,.T.);
#11716=EDGE_CURVE('',#9234,#9237,#2075,.T.);
#11717=EDGE_CURVE('',#9233,#9238,#2076,.T.);
#11718=EDGE_CURVE('',#9237,#9238,#7622,.T.);
#11719=EDGE_CURVE('',#9238,#9231,#2077,.T.);
#11720=EDGE_CURVE('',#9228,#9239,#2078,.T.);
#11721=EDGE_CURVE('',#9240,#9239,#2079,.T.);
#11722=EDGE_CURVE('',#9237,#9240,#2080,.T.);
#11723=EDGE_CURVE('',#9239,#9236,#2081,.T.);
#11724=EDGE_CURVE('',#9235,#9240,#2082,.T.);
#11725=EDGE_CURVE('',#9241,#9242,#2083,.T.);
#11726=EDGE_CURVE('',#9243,#9241,#7623,.T.);
#11727=EDGE_CURVE('',#9244,#9243,#2084,.T.);
#11728=EDGE_CURVE('',#9242,#9244,#7624,.T.);
#11729=EDGE_CURVE('',#9245,#9246,#2085,.T.);
#11730=EDGE_CURVE('',#9247,#9245,#7625,.T.);
#11731=EDGE_CURVE('',#9248,#9247,#2086,.T.);
#11732=EDGE_CURVE('',#9246,#9248,#7626,.T.);
#11733=EDGE_CURVE('',#9249,#9250,#2087,.T.);
#11734=EDGE_CURVE('',#9251,#9249,#7627,.T.);
#11735=EDGE_CURVE('',#9252,#9251,#2088,.T.);
#11736=EDGE_CURVE('',#9250,#9252,#7628,.T.);
#11737=EDGE_CURVE('',#9253,#9254,#2089,.T.);
#11738=EDGE_CURVE('',#9255,#9253,#7629,.T.);
#11739=EDGE_CURVE('',#9256,#9255,#2090,.T.);
#11740=EDGE_CURVE('',#9254,#9256,#7630,.T.);
#11741=EDGE_CURVE('',#9257,#9258,#2091,.T.);
#11742=EDGE_CURVE('',#9259,#9257,#7631,.T.);
#11743=EDGE_CURVE('',#9260,#9259,#2092,.T.);
#11744=EDGE_CURVE('',#9258,#9260,#7632,.T.);
#11745=EDGE_CURVE('',#9261,#9262,#2093,.T.);
#11746=EDGE_CURVE('',#9263,#9261,#7633,.T.);
#11747=EDGE_CURVE('',#9264,#9263,#2094,.T.);
#11748=EDGE_CURVE('',#9262,#9264,#7634,.T.);
#11749=EDGE_CURVE('',#9265,#9266,#2095,.T.);
#11750=EDGE_CURVE('',#9267,#9265,#7635,.T.);
#11751=EDGE_CURVE('',#9268,#9267,#2096,.T.);
#11752=EDGE_CURVE('',#9266,#9268,#7636,.T.);
#11753=EDGE_CURVE('',#9269,#9270,#2097,.T.);
#11754=EDGE_CURVE('',#9271,#9269,#7637,.T.);
#11755=EDGE_CURVE('',#9272,#9271,#2098,.T.);
#11756=EDGE_CURVE('',#9270,#9272,#7638,.T.);
#11757=EDGE_CURVE('',#9273,#9274,#2099,.T.);
#11758=EDGE_CURVE('',#9275,#9273,#7639,.T.);
#11759=EDGE_CURVE('',#9276,#9275,#2100,.T.);
#11760=EDGE_CURVE('',#9274,#9276,#7640,.T.);
#11761=EDGE_CURVE('',#9277,#9278,#2101,.T.);
#11762=EDGE_CURVE('',#9279,#9277,#7641,.T.);
#11763=EDGE_CURVE('',#9280,#9279,#2102,.T.);
#11764=EDGE_CURVE('',#9278,#9280,#7642,.T.);
#11765=EDGE_CURVE('',#9281,#9282,#2103,.T.);
#11766=EDGE_CURVE('',#9283,#9281,#7643,.T.);
#11767=EDGE_CURVE('',#9284,#9283,#2104,.T.);
#11768=EDGE_CURVE('',#9282,#9284,#7644,.T.);
#11769=EDGE_CURVE('',#9285,#9286,#2105,.T.);
#11770=EDGE_CURVE('',#9287,#9285,#7645,.T.);
#11771=EDGE_CURVE('',#9288,#9287,#2106,.T.);
#11772=EDGE_CURVE('',#9286,#9288,#7646,.T.);
#11773=EDGE_CURVE('',#9289,#9290,#2107,.T.);
#11774=EDGE_CURVE('',#9291,#9289,#7647,.T.);
#11775=EDGE_CURVE('',#9292,#9291,#2108,.T.);
#11776=EDGE_CURVE('',#9290,#9292,#7648,.T.);
#11777=EDGE_CURVE('',#9293,#9294,#2109,.T.);
#11778=EDGE_CURVE('',#9295,#9293,#7649,.T.);
#11779=EDGE_CURVE('',#9296,#9295,#2110,.T.);
#11780=EDGE_CURVE('',#9294,#9296,#7650,.T.);
#11781=EDGE_CURVE('',#9297,#9298,#2111,.T.);
#11782=EDGE_CURVE('',#9299,#9297,#7651,.T.);
#11783=EDGE_CURVE('',#9300,#9299,#2112,.T.);
#11784=EDGE_CURVE('',#9298,#9300,#7652,.T.);
#11785=EDGE_CURVE('',#9301,#9302,#2113,.T.);
#11786=EDGE_CURVE('',#9303,#9301,#7653,.T.);
#11787=EDGE_CURVE('',#9304,#9303,#2114,.T.);
#11788=EDGE_CURVE('',#9302,#9304,#7654,.T.);
#11789=EDGE_CURVE('',#9305,#9306,#2115,.T.);
#11790=EDGE_CURVE('',#9307,#9305,#7655,.T.);
#11791=EDGE_CURVE('',#9308,#9307,#2116,.T.);
#11792=EDGE_CURVE('',#9306,#9308,#7656,.T.);
#11793=EDGE_CURVE('',#9309,#9310,#2117,.T.);
#11794=EDGE_CURVE('',#9311,#9309,#7657,.T.);
#11795=EDGE_CURVE('',#9312,#9311,#2118,.T.);
#11796=EDGE_CURVE('',#9310,#9312,#7658,.T.);
#11797=EDGE_CURVE('',#9313,#9314,#2119,.T.);
#11798=EDGE_CURVE('',#9315,#9313,#7659,.T.);
#11799=EDGE_CURVE('',#9316,#9315,#2120,.T.);
#11800=EDGE_CURVE('',#9314,#9316,#7660,.T.);
#11801=EDGE_CURVE('',#9317,#9318,#2121,.T.);
#11802=EDGE_CURVE('',#9319,#9317,#7661,.T.);
#11803=EDGE_CURVE('',#9320,#9319,#2122,.T.);
#11804=EDGE_CURVE('',#9318,#9320,#7662,.T.);
#11805=EDGE_CURVE('',#9321,#9322,#2123,.T.);
#11806=EDGE_CURVE('',#9323,#9321,#7663,.T.);
#11807=EDGE_CURVE('',#9324,#9323,#2124,.T.);
#11808=EDGE_CURVE('',#9322,#9324,#7664,.T.);
#11809=EDGE_CURVE('',#9325,#9326,#2125,.T.);
#11810=EDGE_CURVE('',#9327,#9325,#7665,.T.);
#11811=EDGE_CURVE('',#9328,#9327,#2126,.T.);
#11812=EDGE_CURVE('',#9326,#9328,#7666,.T.);
#11813=EDGE_CURVE('',#9329,#9330,#2127,.T.);
#11814=EDGE_CURVE('',#9331,#9329,#7667,.T.);
#11815=EDGE_CURVE('',#9332,#9331,#2128,.T.);
#11816=EDGE_CURVE('',#9330,#9332,#7668,.T.);
#11817=EDGE_CURVE('',#9333,#9334,#2129,.T.);
#11818=EDGE_CURVE('',#9335,#9333,#7669,.T.);
#11819=EDGE_CURVE('',#9336,#9335,#2130,.T.);
#11820=EDGE_CURVE('',#9334,#9336,#7670,.T.);
#11821=EDGE_CURVE('',#9337,#9338,#2131,.T.);
#11822=EDGE_CURVE('',#9339,#9337,#7671,.T.);
#11823=EDGE_CURVE('',#9340,#9339,#2132,.T.);
#11824=EDGE_CURVE('',#9338,#9340,#7672,.T.);
#11825=EDGE_CURVE('',#9341,#9342,#2133,.T.);
#11826=EDGE_CURVE('',#9343,#9341,#7673,.T.);
#11827=EDGE_CURVE('',#9344,#9343,#2134,.T.);
#11828=EDGE_CURVE('',#9342,#9344,#7674,.T.);
#11829=EDGE_CURVE('',#9345,#9346,#2135,.T.);
#11830=EDGE_CURVE('',#9347,#9345,#7675,.T.);
#11831=EDGE_CURVE('',#9348,#9347,#2136,.T.);
#11832=EDGE_CURVE('',#9346,#9348,#7676,.T.);
#11833=EDGE_CURVE('',#9349,#9350,#2137,.T.);
#11834=EDGE_CURVE('',#9351,#9349,#7677,.T.);
#11835=EDGE_CURVE('',#9352,#9351,#2138,.T.);
#11836=EDGE_CURVE('',#9350,#9352,#7678,.T.);
#11837=EDGE_CURVE('',#9353,#9354,#2139,.T.);
#11838=EDGE_CURVE('',#9355,#9353,#7679,.T.);
#11839=EDGE_CURVE('',#9356,#9355,#2140,.T.);
#11840=EDGE_CURVE('',#9354,#9356,#7680,.T.);
#11841=EDGE_CURVE('',#9357,#9358,#2141,.T.);
#11842=EDGE_CURVE('',#9359,#9357,#7681,.T.);
#11843=EDGE_CURVE('',#9360,#9359,#2142,.T.);
#11844=EDGE_CURVE('',#9358,#9360,#7682,.T.);
#11845=EDGE_CURVE('',#9361,#9362,#2143,.T.);
#11846=EDGE_CURVE('',#9363,#9361,#7683,.T.);
#11847=EDGE_CURVE('',#9364,#9363,#2144,.T.);
#11848=EDGE_CURVE('',#9362,#9364,#7684,.T.);
#11849=EDGE_CURVE('',#9365,#9366,#2145,.T.);
#11850=EDGE_CURVE('',#9367,#9365,#7685,.T.);
#11851=EDGE_CURVE('',#9368,#9367,#2146,.T.);
#11852=EDGE_CURVE('',#9366,#9368,#7686,.T.);
#11853=EDGE_CURVE('',#9369,#9370,#2147,.T.);
#11854=EDGE_CURVE('',#9371,#9369,#7687,.T.);
#11855=EDGE_CURVE('',#9372,#9371,#2148,.T.);
#11856=EDGE_CURVE('',#9370,#9372,#7688,.T.);
#11857=EDGE_CURVE('',#9373,#9374,#2149,.T.);
#11858=EDGE_CURVE('',#9375,#9373,#7689,.T.);
#11859=EDGE_CURVE('',#9376,#9375,#2150,.T.);
#11860=EDGE_CURVE('',#9374,#9376,#7690,.T.);
#11861=EDGE_CURVE('',#9377,#9378,#2151,.T.);
#11862=EDGE_CURVE('',#9379,#9377,#7691,.T.);
#11863=EDGE_CURVE('',#9380,#9379,#2152,.T.);
#11864=EDGE_CURVE('',#9378,#9380,#7692,.T.);
#11865=EDGE_CURVE('',#9381,#9382,#2153,.T.);
#11866=EDGE_CURVE('',#9383,#9381,#7693,.T.);
#11867=EDGE_CURVE('',#9384,#9383,#2154,.T.);
#11868=EDGE_CURVE('',#9382,#9384,#7694,.T.);
#11869=EDGE_CURVE('',#9385,#9386,#2155,.T.);
#11870=EDGE_CURVE('',#9387,#9385,#7695,.T.);
#11871=EDGE_CURVE('',#9388,#9387,#2156,.T.);
#11872=EDGE_CURVE('',#9386,#9388,#7696,.T.);
#11873=EDGE_CURVE('',#9389,#9390,#2157,.T.);
#11874=EDGE_CURVE('',#9391,#9389,#7697,.T.);
#11875=EDGE_CURVE('',#9392,#9391,#2158,.T.);
#11876=EDGE_CURVE('',#9390,#9392,#7698,.T.);
#11877=EDGE_CURVE('',#9393,#9394,#2159,.T.);
#11878=EDGE_CURVE('',#9395,#9393,#7699,.T.);
#11879=EDGE_CURVE('',#9396,#9395,#2160,.T.);
#11880=EDGE_CURVE('',#9394,#9396,#7700,.T.);
#11881=EDGE_CURVE('',#9397,#9398,#2161,.T.);
#11882=EDGE_CURVE('',#9399,#9397,#7701,.T.);
#11883=EDGE_CURVE('',#9400,#9399,#2162,.T.);
#11884=EDGE_CURVE('',#9398,#9400,#7702,.T.);
#11885=EDGE_CURVE('',#9401,#9402,#2163,.T.);
#11886=EDGE_CURVE('',#9403,#9401,#7703,.T.);
#11887=EDGE_CURVE('',#9404,#9403,#2164,.T.);
#11888=EDGE_CURVE('',#9402,#9404,#7704,.T.);
#11889=EDGE_CURVE('',#9405,#9406,#2165,.T.);
#11890=EDGE_CURVE('',#9407,#9405,#7705,.T.);
#11891=EDGE_CURVE('',#9408,#9407,#2166,.T.);
#11892=EDGE_CURVE('',#9406,#9408,#7706,.T.);
#11893=EDGE_CURVE('',#9409,#9410,#2167,.T.);
#11894=EDGE_CURVE('',#9411,#9409,#7707,.T.);
#11895=EDGE_CURVE('',#9412,#9411,#2168,.T.);
#11896=EDGE_CURVE('',#9410,#9412,#7708,.T.);
#11897=EDGE_CURVE('',#9413,#9414,#2169,.T.);
#11898=EDGE_CURVE('',#9415,#9413,#7709,.T.);
#11899=EDGE_CURVE('',#9416,#9415,#2170,.T.);
#11900=EDGE_CURVE('',#9414,#9416,#7710,.T.);
#11901=EDGE_CURVE('',#9241,#9417,#7711,.T.);
#11902=EDGE_CURVE('',#9417,#9418,#7712,.T.);
#11903=EDGE_CURVE('',#9418,#9415,#7713,.T.);
#11904=EDGE_CURVE('',#9413,#9411,#7714,.T.);
#11905=EDGE_CURVE('',#9409,#9407,#7715,.T.);
#11906=EDGE_CURVE('',#9405,#9403,#7716,.T.);
#11907=EDGE_CURVE('',#9401,#9399,#7717,.T.);
#11908=EDGE_CURVE('',#9397,#9395,#7718,.T.);
#11909=EDGE_CURVE('',#9393,#9391,#7719,.T.);
#11910=EDGE_CURVE('',#9389,#9387,#7720,.T.);
#11911=EDGE_CURVE('',#9385,#9383,#7721,.T.);
#11912=EDGE_CURVE('',#9381,#9379,#7722,.T.);
#11913=EDGE_CURVE('',#9377,#9375,#7723,.T.);
#11914=EDGE_CURVE('',#9373,#9371,#7724,.T.);
#11915=EDGE_CURVE('',#9369,#9367,#7725,.T.);
#11916=EDGE_CURVE('',#9365,#9363,#7726,.T.);
#11917=EDGE_CURVE('',#9361,#9359,#7727,.T.);
#11918=EDGE_CURVE('',#9357,#9355,#7728,.T.);
#11919=EDGE_CURVE('',#9353,#9351,#7729,.T.);
#11920=EDGE_CURVE('',#9349,#9347,#7730,.T.);
#11921=EDGE_CURVE('',#9345,#9343,#7731,.T.);
#11922=EDGE_CURVE('',#9341,#9339,#7732,.T.);
#11923=EDGE_CURVE('',#9337,#9335,#7733,.T.);
#11924=EDGE_CURVE('',#9333,#9331,#7734,.T.);
#11925=EDGE_CURVE('',#9329,#9327,#7735,.T.);
#11926=EDGE_CURVE('',#9325,#9323,#7736,.T.);
#11927=EDGE_CURVE('',#9321,#9319,#7737,.T.);
#11928=EDGE_CURVE('',#9317,#9315,#7738,.T.);
#11929=EDGE_CURVE('',#9313,#9311,#7739,.T.);
#11930=EDGE_CURVE('',#9309,#9307,#7740,.T.);
#11931=EDGE_CURVE('',#9305,#9303,#7741,.T.);
#11932=EDGE_CURVE('',#9301,#9299,#7742,.T.);
#11933=EDGE_CURVE('',#9297,#9295,#7743,.T.);
#11934=EDGE_CURVE('',#9293,#9291,#7744,.T.);
#11935=EDGE_CURVE('',#9289,#9287,#7745,.T.);
#11936=EDGE_CURVE('',#9285,#9283,#7746,.T.);
#11937=EDGE_CURVE('',#9281,#9279,#7747,.T.);
#11938=EDGE_CURVE('',#9277,#9275,#7748,.T.);
#11939=EDGE_CURVE('',#9273,#9271,#7749,.T.);
#11940=EDGE_CURVE('',#9269,#9267,#7750,.T.);
#11941=EDGE_CURVE('',#9265,#9263,#7751,.T.);
#11942=EDGE_CURVE('',#9261,#9259,#7752,.T.);
#11943=EDGE_CURVE('',#9257,#9255,#7753,.T.);
#11944=EDGE_CURVE('',#9253,#9251,#7754,.T.);
#11945=EDGE_CURVE('',#9249,#9247,#7755,.T.);
#11946=EDGE_CURVE('',#9245,#9243,#7756,.T.);
#11947=EDGE_CURVE('',#9419,#9419,#7757,.T.);
#11948=EDGE_CURVE('',#9242,#9420,#7758,.T.);
#11949=EDGE_CURVE('',#9420,#9417,#2171,.T.);
#11950=EDGE_CURVE('',#9418,#9421,#2172,.T.);
#11951=EDGE_CURVE('',#9421,#9416,#7759,.T.);
#11952=EDGE_CURVE('',#9414,#9412,#7760,.T.);
#11953=EDGE_CURVE('',#9410,#9408,#7761,.T.);
#11954=EDGE_CURVE('',#9406,#9404,#7762,.T.);
#11955=EDGE_CURVE('',#9402,#9400,#7763,.T.);
#11956=EDGE_CURVE('',#9398,#9396,#7764,.T.);
#11957=EDGE_CURVE('',#9394,#9392,#7765,.T.);
#11958=EDGE_CURVE('',#9390,#9388,#7766,.T.);
#11959=EDGE_CURVE('',#9386,#9384,#7767,.T.);
#11960=EDGE_CURVE('',#9382,#9380,#7768,.T.);
#11961=EDGE_CURVE('',#9378,#9376,#7769,.T.);
#11962=EDGE_CURVE('',#9374,#9372,#7770,.T.);
#11963=EDGE_CURVE('',#9370,#9368,#7771,.T.);
#11964=EDGE_CURVE('',#9366,#9364,#7772,.T.);
#11965=EDGE_CURVE('',#9362,#9360,#7773,.T.);
#11966=EDGE_CURVE('',#9358,#9356,#7774,.T.);
#11967=EDGE_CURVE('',#9354,#9352,#7775,.T.);
#11968=EDGE_CURVE('',#9350,#9348,#7776,.T.);
#11969=EDGE_CURVE('',#9346,#9344,#7777,.T.);
#11970=EDGE_CURVE('',#9342,#9340,#7778,.T.);
#11971=EDGE_CURVE('',#9338,#9336,#7779,.T.);
#11972=EDGE_CURVE('',#9334,#9332,#7780,.T.);
#11973=EDGE_CURVE('',#9330,#9328,#7781,.T.);
#11974=EDGE_CURVE('',#9326,#9324,#7782,.T.);
#11975=EDGE_CURVE('',#9322,#9320,#7783,.T.);
#11976=EDGE_CURVE('',#9318,#9316,#7784,.T.);
#11977=EDGE_CURVE('',#9314,#9312,#7785,.T.);
#11978=EDGE_CURVE('',#9310,#9308,#7786,.T.);
#11979=EDGE_CURVE('',#9306,#9304,#7787,.T.);
#11980=EDGE_CURVE('',#9302,#9300,#7788,.T.);
#11981=EDGE_CURVE('',#9298,#9296,#7789,.T.);
#11982=EDGE_CURVE('',#9294,#9292,#7790,.T.);
#11983=EDGE_CURVE('',#9290,#9288,#7791,.T.);
#11984=EDGE_CURVE('',#9286,#9284,#7792,.T.);
#11985=EDGE_CURVE('',#9282,#9280,#7793,.T.);
#11986=EDGE_CURVE('',#9278,#9276,#7794,.T.);
#11987=EDGE_CURVE('',#9274,#9272,#7795,.T.);
#11988=EDGE_CURVE('',#9270,#9268,#7796,.T.);
#11989=EDGE_CURVE('',#9266,#9264,#7797,.T.);
#11990=EDGE_CURVE('',#9262,#9260,#7798,.T.);
#11991=EDGE_CURVE('',#9258,#9256,#7799,.T.);
#11992=EDGE_CURVE('',#9254,#9252,#7800,.T.);
#11993=EDGE_CURVE('',#9250,#9248,#7801,.T.);
#11994=EDGE_CURVE('',#9421,#9420,#7802,.T.);
#11995=EDGE_CURVE('',#9246,#9244,#7803,.T.);
#11996=EDGE_CURVE('',#9422,#9422,#7804,.T.);
#11997=EDGE_CURVE('',#9422,#9419,#2173,.T.);
#11998=EDGE_CURVE('',#9423,#9424,#7805,.T.);
#11999=EDGE_CURVE('',#9424,#9425,#7806,.T.);
#12000=EDGE_CURVE('',#9425,#9425,#7807,.T.);
#12001=EDGE_CURVE('',#9424,#9423,#7808,.T.);
#12002=EDGE_CURVE('',#9426,#9427,#7809,.T.);
#12003=EDGE_CURVE('',#9426,#9423,#2174,.T.);
#12004=EDGE_CURVE('',#9427,#9426,#7810,.T.);
#12005=EDGE_CURVE('',#9428,#9428,#7811,.T.);
#12006=EDGE_CURVE('',#9429,#9429,#7812,.T.);
#12007=EDGE_CURVE('',#9429,#9427,#7813,.T.);
#12008=EDGE_CURVE('',#9430,#9430,#7814,.T.);
#12009=EDGE_CURVE('',#9428,#9430,#2175,.T.);
#12010=EDGE_CURVE('',#9431,#9432,#7815,.T.);
#12011=EDGE_CURVE('',#9432,#9433,#2176,.T.);
#12012=EDGE_CURVE('',#9433,#9434,#7816,.T.);
#12013=EDGE_CURVE('',#9434,#9431,#2177,.T.);
#12014=EDGE_CURVE('',#9435,#9432,#7817,.T.);
#12015=EDGE_CURVE('',#9436,#9435,#2178,.T.);
#12016=EDGE_CURVE('',#9433,#9436,#7818,.T.);
#12017=EDGE_CURVE('',#9435,#9437,#7819,.T.);
#12018=EDGE_CURVE('',#9437,#9438,#2179,.T.);
#12019=EDGE_CURVE('',#9438,#9436,#7820,.T.);
#12020=EDGE_CURVE('',#9439,#9437,#2180,.T.);
#12021=EDGE_CURVE('',#9440,#9439,#2181,.T.);
#12022=EDGE_CURVE('',#9438,#9440,#2182,.T.);
#12023=EDGE_CURVE('',#9441,#9442,#7821,.T.);
#12024=EDGE_CURVE('',#9442,#9443,#2183,.T.);
#12025=EDGE_CURVE('',#9443,#9444,#7822,.T.);
#12026=EDGE_CURVE('',#9444,#9441,#2184,.T.);
#12027=EDGE_CURVE('',#9445,#9442,#7823,.T.);
#12028=EDGE_CURVE('',#9446,#9445,#2185,.T.);
#12029=EDGE_CURVE('',#9443,#9446,#7824,.T.);
#12030=EDGE_CURVE('',#9445,#9447,#7825,.T.);
#12031=EDGE_CURVE('',#9447,#9448,#2186,.T.);
#12032=EDGE_CURVE('',#9448,#9446,#7826,.T.);
#12033=EDGE_CURVE('',#9449,#9447,#2187,.T.);
#12034=EDGE_CURVE('',#9450,#9449,#2188,.T.);
#12035=EDGE_CURVE('',#9448,#9450,#2189,.T.);
#12036=EDGE_CURVE('',#9451,#9452,#7827,.T.);
#12037=EDGE_CURVE('',#9452,#9453,#2190,.T.);
#12038=EDGE_CURVE('',#9453,#9454,#7828,.T.);
#12039=EDGE_CURVE('',#9454,#9451,#2191,.T.);
#12040=EDGE_CURVE('',#9455,#9452,#7829,.T.);
#12041=EDGE_CURVE('',#9456,#9455,#2192,.T.);
#12042=EDGE_CURVE('',#9453,#9456,#7830,.T.);
#12043=EDGE_CURVE('',#9455,#9457,#7831,.T.);
#12044=EDGE_CURVE('',#9457,#9458,#2193,.T.);
#12045=EDGE_CURVE('',#9458,#9456,#7832,.T.);
#12046=EDGE_CURVE('',#9459,#9457,#2194,.T.);
#12047=EDGE_CURVE('',#9460,#9459,#2195,.T.);
#12048=EDGE_CURVE('',#9458,#9460,#2196,.T.);
#12049=EDGE_CURVE('',#9461,#9462,#7833,.T.);
#12050=EDGE_CURVE('',#9462,#9463,#2197,.T.);
#12051=EDGE_CURVE('',#9463,#9464,#7834,.T.);
#12052=EDGE_CURVE('',#9464,#9461,#2198,.T.);
#12053=EDGE_CURVE('',#9465,#9462,#7835,.T.);
#12054=EDGE_CURVE('',#9466,#9465,#2199,.T.);
#12055=EDGE_CURVE('',#9463,#9466,#7836,.T.);
#12056=EDGE_CURVE('',#9465,#9467,#7837,.T.);
#12057=EDGE_CURVE('',#9467,#9468,#2200,.T.);
#12058=EDGE_CURVE('',#9468,#9466,#7838,.T.);
#12059=EDGE_CURVE('',#9469,#9467,#2201,.T.);
#12060=EDGE_CURVE('',#9470,#9469,#2202,.T.);
#12061=EDGE_CURVE('',#9468,#9470,#2203,.T.);
#12062=EDGE_CURVE('',#9471,#9472,#7839,.T.);
#12063=EDGE_CURVE('',#9472,#9473,#2204,.T.);
#12064=EDGE_CURVE('',#9473,#9474,#7840,.T.);
#12065=EDGE_CURVE('',#9474,#9471,#2205,.T.);
#12066=EDGE_CURVE('',#9475,#9472,#7841,.T.);
#12067=EDGE_CURVE('',#9476,#9475,#2206,.T.);
#12068=EDGE_CURVE('',#9473,#9476,#7842,.T.);
#12069=EDGE_CURVE('',#9475,#9477,#7843,.T.);
#12070=EDGE_CURVE('',#9477,#9478,#2207,.T.);
#12071=EDGE_CURVE('',#9478,#9476,#7844,.T.);
#12072=EDGE_CURVE('',#9479,#9477,#2208,.T.);
#12073=EDGE_CURVE('',#9480,#9479,#2209,.T.);
#12074=EDGE_CURVE('',#9478,#9480,#2210,.T.);
#12075=EDGE_CURVE('',#9481,#9474,#2211,.T.);
#12076=EDGE_CURVE('',#9482,#9481,#2212,.T.);
#12077=EDGE_CURVE('',#9471,#9482,#2213,.T.);
#12078=EDGE_CURVE('',#9483,#9464,#2214,.T.);
#12079=EDGE_CURVE('',#9484,#9483,#2215,.T.);
#12080=EDGE_CURVE('',#9461,#9484,#2216,.T.);
#12081=EDGE_CURVE('',#9485,#9444,#2217,.T.);
#12082=EDGE_CURVE('',#9486,#9485,#2218,.T.);
#12083=EDGE_CURVE('',#9441,#9486,#2219,.T.);
#12084=EDGE_CURVE('',#9487,#9434,#2220,.T.);
#12085=EDGE_CURVE('',#9488,#9487,#2221,.T.);
#12086=EDGE_CURVE('',#9431,#9488,#2222,.T.);
#12087=EDGE_CURVE('',#9489,#9479,#7845,.T.);
#12088=EDGE_CURVE('',#9489,#9490,#2223,.T.);
#12089=EDGE_CURVE('',#9480,#9490,#7846,.T.);
#12090=EDGE_CURVE('',#9460,#9483,#7847,.T.);
#12091=EDGE_CURVE('',#9484,#9459,#7848,.T.);
#12092=EDGE_CURVE('',#9490,#9491,#2224,.T.);
#12093=EDGE_CURVE('',#9491,#9492,#7849,.T.);
#12094=EDGE_CURVE('',#9492,#9493,#2225,.T.);
#12095=EDGE_CURVE('',#9493,#9487,#7850,.T.);
#12096=EDGE_CURVE('',#9440,#9485,#7851,.T.);
#12097=EDGE_CURVE('',#9450,#9494,#7852,.T.);
#12098=EDGE_CURVE('',#9494,#9454,#2226,.T.);
#12099=EDGE_CURVE('',#9470,#9481,#7853,.T.);
#12100=EDGE_CURVE('',#9495,#9449,#7854,.T.);
#12101=EDGE_CURVE('',#9495,#9494,#2227,.T.);
#12102=EDGE_CURVE('',#9493,#9496,#2228,.T.);
#12103=EDGE_CURVE('',#9488,#9496,#7855,.T.);
#12104=EDGE_CURVE('',#9451,#9495,#2229,.T.);
#12105=EDGE_CURVE('',#9482,#9469,#7856,.T.);
#12106=EDGE_CURVE('',#9497,#9489,#2230,.T.);
#12107=EDGE_CURVE('',#9491,#9497,#2231,.T.);
#12108=EDGE_CURVE('',#9498,#9497,#7857,.T.);
#12109=EDGE_CURVE('',#9492,#9498,#2232,.T.);
#12110=EDGE_CURVE('',#9496,#9498,#2233,.T.);
#12111=EDGE_CURVE('',#9486,#9439,#7858,.T.);
#12112=EDGE_CURVE('',#9499,#9500,#2234,.T.);
#12113=EDGE_CURVE('',#9500,#9501,#2235,.T.);
#12114=EDGE_CURVE('',#9501,#9502,#2236,.T.);
#12115=EDGE_CURVE('',#9499,#9502,#2237,.T.);
#12116=EDGE_CURVE('',#9503,#9504,#2238,.T.);
#12117=EDGE_CURVE('',#9503,#9505,#2239,.T.);
#12118=EDGE_CURVE('',#9505,#9506,#2240,.T.);
#12119=EDGE_CURVE('',#9504,#9506,#2241,.T.);
#12120=EDGE_CURVE('',#9506,#9501,#2242,.T.);
#12121=EDGE_CURVE('',#9502,#9505,#2243,.T.);
#12122=EDGE_CURVE('',#9507,#9504,#7859,.T.);
#12123=EDGE_CURVE('',#9500,#9508,#2244,.T.);
#12124=EDGE_CURVE('',#9509,#9508,#2245,.T.);
#12125=EDGE_CURVE('',#9507,#9509,#2246,.T.);
#12126=EDGE_CURVE('',#9510,#9507,#2247,.T.);
#12127=EDGE_CURVE('',#9510,#9503,#7860,.T.);
#12128=EDGE_CURVE('',#9511,#9510,#2248,.T.);
#12129=EDGE_CURVE('',#9512,#9511,#2249,.T.);
#12130=EDGE_CURVE('',#9499,#9512,#2250,.T.);
#12131=EDGE_CURVE('',#9508,#9512,#2251,.T.);
#12132=EDGE_CURVE('',#9511,#9509,#2252,.T.);
#12133=EDGE_CURVE('',#9513,#9514,#2253,.T.);
#12134=EDGE_CURVE('',#9514,#9515,#7861,.T.);
#12135=EDGE_CURVE('',#9516,#9515,#2254,.T.);
#12136=EDGE_CURVE('',#9516,#9513,#7862,.T.);
#12137=EDGE_CURVE('',#9517,#9518,#2255,.T.);
#12138=EDGE_CURVE('',#9514,#9518,#2256,.T.);
#12139=EDGE_CURVE('',#9517,#9513,#2257,.T.);
#12140=EDGE_CURVE('',#9519,#9520,#2258,.T.);
#12141=EDGE_CURVE('',#9520,#9518,#7863,.T.);
#12142=EDGE_CURVE('',#9517,#9519,#7864,.T.);
#12143=EDGE_CURVE('',#9521,#9522,#2259,.T.);
#12144=EDGE_CURVE('',#9520,#9522,#7865,.T.);
#12145=EDGE_CURVE('',#9521,#9519,#7866,.T.);
#12146=EDGE_CURVE('',#9523,#9524,#2260,.T.);
#12147=EDGE_CURVE('',#9524,#9522,#7867,.T.);
#12148=EDGE_CURVE('',#9521,#9523,#7868,.T.);
#12149=EDGE_CURVE('',#9525,#9526,#2261,.T.);
#12150=EDGE_CURVE('',#9524,#9526,#2262,.T.);
#12151=EDGE_CURVE('',#9525,#9523,#2263,.T.);
#12152=EDGE_CURVE('',#9527,#9528,#2264,.T.);
#12153=EDGE_CURVE('',#9528,#9526,#7869,.T.);
#12154=EDGE_CURVE('',#9525,#9527,#7870,.T.);
#12155=EDGE_CURVE('',#9529,#9530,#2265,.T.);
#12156=EDGE_CURVE('',#9528,#9529,#7871,.T.);
#12157=EDGE_CURVE('',#9530,#9527,#7872,.T.);
#12158=EDGE_CURVE('',#9531,#9532,#2266,.T.);
#12159=EDGE_CURVE('',#9532,#9533,#7873,.T.);
#12160=EDGE_CURVE('',#9534,#9533,#2267,.T.);
#12161=EDGE_CURVE('',#9534,#9531,#7874,.T.);
#12162=EDGE_CURVE('',#9535,#9533,#2268,.T.);
#12163=EDGE_CURVE('',#9536,#9535,#2269,.T.);
#12164=EDGE_CURVE('',#9534,#9536,#2270,.T.);
#12165=EDGE_CURVE('',#9535,#9537,#7875,.T.);
#12166=EDGE_CURVE('',#9538,#9537,#2271,.T.);
#12167=EDGE_CURVE('',#9538,#9536,#7876,.T.);
#12168=EDGE_CURVE('',#9539,#9537,#7877,.T.);
#12169=EDGE_CURVE('',#9540,#9539,#2272,.T.);
#12170=EDGE_CURVE('',#9538,#9540,#7878,.T.);
#12171=EDGE_CURVE('',#9539,#9541,#7879,.T.);
#12172=EDGE_CURVE('',#9542,#9541,#2273,.T.);
#12173=EDGE_CURVE('',#9542,#9540,#7880,.T.);
#12174=EDGE_CURVE('',#9543,#9541,#2274,.T.);
#12175=EDGE_CURVE('',#9544,#9543,#2275,.T.);
#12176=EDGE_CURVE('',#9542,#9544,#2276,.T.);
#12177=EDGE_CURVE('',#9543,#9529,#7881,.T.);
#12178=EDGE_CURVE('',#9530,#9544,#7882,.T.);
#12179=EDGE_CURVE('',#9532,#9515,#7883,.T.);
#12180=EDGE_CURVE('',#9545,#9545,#7884,.T.);
#12181=EDGE_CURVE('',#9546,#9546,#7885,.T.);
#12182=EDGE_CURVE('',#9547,#9547,#7886,.T.);
#12183=EDGE_CURVE('',#9548,#9548,#7887,.T.);
#12184=EDGE_CURVE('',#9549,#9550,#2277,.T.);
#12185=EDGE_CURVE('',#9550,#9551,#2278,.T.);
#12186=EDGE_CURVE('',#9551,#9552,#2279,.T.);
#12187=EDGE_CURVE('',#9552,#9553,#2280,.T.);
#12188=EDGE_CURVE('',#9553,#9554,#2281,.T.);
#12189=EDGE_CURVE('',#9554,#9555,#2282,.T.);
#12190=EDGE_CURVE('',#9555,#9556,#2283,.T.);
#12191=EDGE_CURVE('',#9556,#9549,#2284,.T.);
#12192=EDGE_CURVE('',#9516,#9531,#7888,.T.);
#12193=EDGE_CURVE('',#9545,#9557,#2285,.T.);
#12194=EDGE_CURVE('',#9557,#9557,#7889,.T.);
#12195=EDGE_CURVE('',#9546,#9558,#2286,.T.);
#12196=EDGE_CURVE('',#9558,#9558,#7890,.T.);
#12197=EDGE_CURVE('',#9547,#9559,#2287,.T.);
#12198=EDGE_CURVE('',#9559,#9559,#7891,.T.);
#12199=EDGE_CURVE('',#9548,#9560,#2288,.T.);
#12200=EDGE_CURVE('',#9560,#9560,#7892,.T.);
#12201=EDGE_CURVE('',#9561,#9550,#2289,.T.);
#12202=EDGE_CURVE('',#9562,#9561,#2290,.T.);
#12203=EDGE_CURVE('',#9551,#9562,#2291,.T.);
#12204=EDGE_CURVE('',#9563,#9562,#2292,.T.);
#12205=EDGE_CURVE('',#9552,#9563,#2293,.T.);
#12206=EDGE_CURVE('',#9564,#9563,#2294,.T.);
#12207=EDGE_CURVE('',#9553,#9564,#2295,.T.);
#12208=EDGE_CURVE('',#9565,#9564,#2296,.T.);
#12209=EDGE_CURVE('',#9554,#9565,#2297,.T.);
#12210=EDGE_CURVE('',#9566,#9565,#2298,.T.);
#12211=EDGE_CURVE('',#9555,#9566,#2299,.T.);
#12212=EDGE_CURVE('',#9567,#9566,#2300,.T.);
#12213=EDGE_CURVE('',#9556,#9567,#2301,.T.);
#12214=EDGE_CURVE('',#9568,#9567,#2302,.T.);
#12215=EDGE_CURVE('',#9549,#9568,#2303,.T.);
#12216=EDGE_CURVE('',#9561,#9568,#2304,.T.);
#12217=EDGE_CURVE('',#9569,#9570,#7893,.T.);
#12218=EDGE_CURVE('',#9570,#9571,#2305,.T.);
#12219=EDGE_CURVE('',#9571,#9572,#7894,.T.);
#12220=EDGE_CURVE('',#9572,#9569,#2306,.T.);
#12221=EDGE_CURVE('',#9573,#9570,#7895,.T.);
#12222=EDGE_CURVE('',#9574,#9573,#2307,.T.);
#12223=EDGE_CURVE('',#9571,#9574,#7896,.T.);
#12224=EDGE_CURVE('',#9573,#9575,#7897,.T.);
#12225=EDGE_CURVE('',#9575,#9576,#2308,.T.);
#12226=EDGE_CURVE('',#9576,#9574,#7898,.T.);
#12227=EDGE_CURVE('',#9577,#9575,#2309,.T.);
#12228=EDGE_CURVE('',#9578,#9577,#2310,.T.);
#12229=EDGE_CURVE('',#9576,#9578,#2311,.T.);
#12230=EDGE_CURVE('',#9579,#9580,#7899,.T.);
#12231=EDGE_CURVE('',#9580,#9581,#2312,.T.);
#12232=EDGE_CURVE('',#9581,#9582,#7900,.T.);
#12233=EDGE_CURVE('',#9582,#9579,#2313,.T.);
#12234=EDGE_CURVE('',#9583,#9580,#7901,.T.);
#12235=EDGE_CURVE('',#9584,#9583,#2314,.T.);
#12236=EDGE_CURVE('',#9581,#9584,#7902,.T.);
#12237=EDGE_CURVE('',#9583,#9585,#7903,.T.);
#12238=EDGE_CURVE('',#9585,#9586,#2315,.T.);
#12239=EDGE_CURVE('',#9586,#9584,#7904,.T.);
#12240=EDGE_CURVE('',#9587,#9585,#2316,.T.);
#12241=EDGE_CURVE('',#9588,#9587,#2317,.T.);
#12242=EDGE_CURVE('',#9586,#9588,#2318,.T.);
#12243=EDGE_CURVE('',#9589,#9590,#7905,.T.);
#12244=EDGE_CURVE('',#9590,#9591,#2319,.T.);
#12245=EDGE_CURVE('',#9591,#9592,#7906,.T.);
#12246=EDGE_CURVE('',#9592,#9589,#2320,.T.);
#12247=EDGE_CURVE('',#9593,#9590,#7907,.T.);
#12248=EDGE_CURVE('',#9594,#9593,#2321,.T.);
#12249=EDGE_CURVE('',#9591,#9594,#7908,.T.);
#12250=EDGE_CURVE('',#9593,#9595,#7909,.T.);
#12251=EDGE_CURVE('',#9595,#9596,#2322,.T.);
#12252=EDGE_CURVE('',#9596,#9594,#7910,.T.);
#12253=EDGE_CURVE('',#9597,#9595,#2323,.T.);
#12254=EDGE_CURVE('',#9598,#9597,#2324,.T.);
#12255=EDGE_CURVE('',#9596,#9598,#2325,.T.);
#12256=EDGE_CURVE('',#9599,#9600,#7911,.T.);
#12257=EDGE_CURVE('',#9600,#9601,#2326,.T.);
#12258=EDGE_CURVE('',#9601,#9602,#7912,.T.);
#12259=EDGE_CURVE('',#9602,#9599,#2327,.T.);
#12260=EDGE_CURVE('',#9603,#9600,#7913,.T.);
#12261=EDGE_CURVE('',#9604,#9603,#2328,.T.);
#12262=EDGE_CURVE('',#9601,#9604,#7914,.T.);
#12263=EDGE_CURVE('',#9603,#9605,#7915,.T.);
#12264=EDGE_CURVE('',#9605,#9606,#2329,.T.);
#12265=EDGE_CURVE('',#9606,#9604,#7916,.T.);
#12266=EDGE_CURVE('',#9607,#9605,#2330,.T.);
#12267=EDGE_CURVE('',#9608,#9607,#2331,.T.);
#12268=EDGE_CURVE('',#9606,#9608,#2332,.T.);
#12269=EDGE_CURVE('',#9609,#9610,#7917,.T.);
#12270=EDGE_CURVE('',#9610,#9611,#2333,.T.);
#12271=EDGE_CURVE('',#9611,#9612,#7918,.T.);
#12272=EDGE_CURVE('',#9612,#9609,#2334,.T.);
#12273=EDGE_CURVE('',#9613,#9610,#7919,.T.);
#12274=EDGE_CURVE('',#9614,#9613,#2335,.T.);
#12275=EDGE_CURVE('',#9611,#9614,#7920,.T.);
#12276=EDGE_CURVE('',#9613,#9615,#7921,.T.);
#12277=EDGE_CURVE('',#9615,#9616,#2336,.T.);
#12278=EDGE_CURVE('',#9616,#9614,#7922,.T.);
#12279=EDGE_CURVE('',#9617,#9615,#2337,.T.);
#12280=EDGE_CURVE('',#9618,#9617,#2338,.T.);
#12281=EDGE_CURVE('',#9616,#9618,#2339,.T.);
#12282=EDGE_CURVE('',#9619,#9612,#2340,.T.);
#12283=EDGE_CURVE('',#9620,#9619,#2341,.T.);
#12284=EDGE_CURVE('',#9609,#9620,#2342,.T.);
#12285=EDGE_CURVE('',#9621,#9602,#2343,.T.);
#12286=EDGE_CURVE('',#9622,#9621,#2344,.T.);
#12287=EDGE_CURVE('',#9599,#9622,#2345,.T.);
#12288=EDGE_CURVE('',#9623,#9582,#2346,.T.);
#12289=EDGE_CURVE('',#9624,#9623,#2347,.T.);
#12290=EDGE_CURVE('',#9579,#9624,#2348,.T.);
#12291=EDGE_CURVE('',#9625,#9572,#2349,.T.);
#12292=EDGE_CURVE('',#9626,#9625,#2350,.T.);
#12293=EDGE_CURVE('',#9569,#9626,#2351,.T.);
#12294=EDGE_CURVE('',#9627,#9617,#7923,.T.);
#12295=EDGE_CURVE('',#9628,#9627,#2352,.T.);
#12296=EDGE_CURVE('',#9618,#9628,#7924,.T.);
#12297=EDGE_CURVE('',#9598,#9621,#7925,.T.);
#12298=EDGE_CURVE('',#9622,#9597,#7926,.T.);
#12299=EDGE_CURVE('',#9628,#9629,#2353,.T.);
#12300=EDGE_CURVE('',#9629,#9630,#7927,.T.);
#12301=EDGE_CURVE('',#9630,#9631,#2354,.T.);
#12302=EDGE_CURVE('',#9631,#9625,#7928,.T.);
#12303=EDGE_CURVE('',#9578,#9623,#7929,.T.);
#12304=EDGE_CURVE('',#9588,#9632,#7930,.T.);
#12305=EDGE_CURVE('',#9632,#9592,#2355,.T.);
#12306=EDGE_CURVE('',#9608,#9619,#7931,.T.);
#12307=EDGE_CURVE('',#9633,#9587,#7932,.T.);
#12308=EDGE_CURVE('',#9633,#9632,#2356,.T.);
#12309=EDGE_CURVE('',#9631,#9634,#2357,.T.);
#12310=EDGE_CURVE('',#9626,#9634,#7933,.T.);
#12311=EDGE_CURVE('',#9589,#9633,#2358,.T.);
#12312=EDGE_CURVE('',#9620,#9607,#7934,.T.);
#12313=EDGE_CURVE('',#9635,#9629,#2359,.T.);
#12314=EDGE_CURVE('',#9636,#9635,#7935,.T.);
#12315=EDGE_CURVE('',#9630,#9636,#2360,.T.);
#12316=EDGE_CURVE('',#9634,#9636,#2361,.T.);
#12317=EDGE_CURVE('',#9624,#9577,#7936,.T.);
#12318=EDGE_CURVE('',#9635,#9627,#2362,.T.);
#12319=EDGE_CURVE('',#9637,#9638,#2363,.T.);
#12320=EDGE_CURVE('',#9639,#9637,#2364,.T.);
#12321=EDGE_CURVE('',#9640,#9639,#2365,.T.);
#12322=EDGE_CURVE('',#9640,#9638,#2366,.T.);
#12323=EDGE_CURVE('',#9638,#9641,#2367,.T.);
#12324=EDGE_CURVE('',#9642,#9640,#2368,.T.);
#12325=EDGE_CURVE('',#9642,#9641,#2369,.T.);
#12326=EDGE_CURVE('',#9641,#9643,#2370,.T.);
#12327=EDGE_CURVE('',#9644,#9642,#2371,.T.);
#12328=EDGE_CURVE('',#9644,#9643,#2372,.T.);
#12329=EDGE_CURVE('',#9643,#9637,#2373,.T.);
#12330=EDGE_CURVE('',#9639,#9644,#2374,.T.);
#12331=EDGE_CURVE('',#9645,#9646,#2375,.T.);
#12332=EDGE_CURVE('',#9647,#9645,#2376,.T.);
#12333=EDGE_CURVE('',#9648,#9647,#2377,.T.);
#12334=EDGE_CURVE('',#9648,#9646,#2378,.T.);
#12335=EDGE_CURVE('',#9646,#9649,#2379,.T.);
#12336=EDGE_CURVE('',#9650,#9648,#2380,.T.);
#12337=EDGE_CURVE('',#9650,#9649,#2381,.T.);
#12338=EDGE_CURVE('',#9649,#9651,#2382,.T.);
#12339=EDGE_CURVE('',#9652,#9650,#2383,.T.);
#12340=EDGE_CURVE('',#9652,#9651,#2384,.T.);
#12341=EDGE_CURVE('',#9651,#9645,#2385,.T.);
#12342=EDGE_CURVE('',#9647,#9652,#2386,.T.);
#12343=EDGE_CURVE('',#9653,#9654,#2387,.T.);
#12344=EDGE_CURVE('',#9655,#9653,#2388,.T.);
#12345=EDGE_CURVE('',#9656,#9655,#2389,.T.);
#12346=EDGE_CURVE('',#9656,#9654,#2390,.T.);
#12347=EDGE_CURVE('',#9654,#9657,#2391,.T.);
#12348=EDGE_CURVE('',#9658,#9656,#2392,.T.);
#12349=EDGE_CURVE('',#9658,#9657,#2393,.T.);
#12350=EDGE_CURVE('',#9657,#9659,#2394,.T.);
#12351=EDGE_CURVE('',#9660,#9658,#2395,.T.);
#12352=EDGE_CURVE('',#9660,#9659,#2396,.T.);
#12353=EDGE_CURVE('',#9659,#9653,#2397,.T.);
#12354=EDGE_CURVE('',#9655,#9660,#2398,.T.);
#12355=EDGE_CURVE('',#9661,#9662,#2399,.T.);
#12356=EDGE_CURVE('',#9663,#9661,#2400,.T.);
#12357=EDGE_CURVE('',#9664,#9663,#2401,.T.);
#12358=EDGE_CURVE('',#9664,#9662,#2402,.T.);
#12359=EDGE_CURVE('',#9662,#9665,#2403,.T.);
#12360=EDGE_CURVE('',#9666,#9664,#2404,.T.);
#12361=EDGE_CURVE('',#9666,#9665,#2405,.T.);
#12362=EDGE_CURVE('',#9665,#9667,#2406,.T.);
#12363=EDGE_CURVE('',#9668,#9666,#2407,.T.);
#12364=EDGE_CURVE('',#9668,#9667,#2408,.T.);
#12365=EDGE_CURVE('',#9667,#9661,#2409,.T.);
#12366=EDGE_CURVE('',#9663,#9668,#2410,.T.);
#12367=EDGE_CURVE('',#9669,#9670,#2411,.T.);
#12368=EDGE_CURVE('',#9671,#9669,#2412,.T.);
#12369=EDGE_CURVE('',#9672,#9671,#2413,.T.);
#12370=EDGE_CURVE('',#9672,#9670,#2414,.T.);
#12371=EDGE_CURVE('',#9670,#9673,#2415,.T.);
#12372=EDGE_CURVE('',#9674,#9672,#2416,.T.);
#12373=EDGE_CURVE('',#9674,#9673,#2417,.T.);
#12374=EDGE_CURVE('',#9673,#9675,#2418,.T.);
#12375=EDGE_CURVE('',#9676,#9674,#2419,.T.);
#12376=EDGE_CURVE('',#9676,#9675,#2420,.T.);
#12377=EDGE_CURVE('',#9675,#9669,#2421,.T.);
#12378=EDGE_CURVE('',#9671,#9676,#2422,.T.);
#12379=EDGE_CURVE('',#9677,#9678,#2423,.T.);
#12380=EDGE_CURVE('',#9679,#9677,#2424,.T.);
#12381=EDGE_CURVE('',#9680,#9679,#2425,.T.);
#12382=EDGE_CURVE('',#9680,#9678,#2426,.T.);
#12383=EDGE_CURVE('',#9678,#9681,#2427,.T.);
#12384=EDGE_CURVE('',#9682,#9680,#2428,.T.);
#12385=EDGE_CURVE('',#9682,#9681,#2429,.T.);
#12386=EDGE_CURVE('',#9681,#9683,#2430,.T.);
#12387=EDGE_CURVE('',#9684,#9682,#2431,.T.);
#12388=EDGE_CURVE('',#9684,#9683,#2432,.T.);
#12389=EDGE_CURVE('',#9683,#9677,#2433,.T.);
#12390=EDGE_CURVE('',#9679,#9684,#2434,.T.);
#12391=EDGE_CURVE('',#9685,#9686,#2435,.T.);
#12392=EDGE_CURVE('',#9687,#9685,#2436,.T.);
#12393=EDGE_CURVE('',#9687,#9688,#2437,.T.);
#12394=EDGE_CURVE('',#9686,#9688,#2438,.T.);
#12395=EDGE_CURVE('',#9689,#9687,#2439,.T.);
#12396=EDGE_CURVE('',#9690,#9689,#2440,.T.);
#12397=EDGE_CURVE('',#9688,#9690,#2441,.T.);
#12398=EDGE_CURVE('',#9685,#9691,#2442,.T.);
#12399=EDGE_CURVE('',#9692,#9686,#2443,.T.);
#12400=EDGE_CURVE('',#9691,#9692,#2444,.T.);
#12401=EDGE_CURVE('',#9693,#9690,#2445,.T.);
#12402=EDGE_CURVE('',#9694,#9693,#2446,.T.);
#12403=EDGE_CURVE('',#9695,#9694,#2447,.T.);
#12404=EDGE_CURVE('',#9695,#9696,#2448,.T.);
#12405=EDGE_CURVE('',#9692,#9696,#2449,.T.);
#12406=EDGE_CURVE('',#9697,#9689,#2450,.T.);
#12407=EDGE_CURVE('',#9697,#9698,#2451,.T.);
#12408=EDGE_CURVE('',#9699,#9698,#2452,.T.);
#12409=EDGE_CURVE('',#9699,#9693,#2453,.T.);
#12410=EDGE_CURVE('',#9700,#9695,#2454,.T.);
#12411=EDGE_CURVE('',#9701,#9700,#2455,.T.);
#12412=EDGE_CURVE('',#9696,#9701,#2456,.T.);
#12413=EDGE_CURVE('',#9702,#9694,#2457,.T.);
#12414=EDGE_CURVE('',#9702,#9703,#2458,.T.);
#12415=EDGE_CURVE('',#9703,#9704,#2459,.T.);
#12416=EDGE_CURVE('',#9704,#9705,#2460,.T.);
#12417=EDGE_CURVE('',#9706,#9705,#2461,.T.);
#12418=EDGE_CURVE('',#9706,#9707,#2462,.T.);
#12419=EDGE_CURVE('',#9707,#9708,#2463,.T.);
#12420=EDGE_CURVE('',#9708,#9709,#2464,.T.);
#12421=EDGE_CURVE('',#9710,#9709,#2465,.T.);
#12422=EDGE_CURVE('',#9700,#9710,#2466,.T.);
#12423=EDGE_CURVE('',#9711,#9712,#2467,.T.);
#12424=EDGE_CURVE('',#9712,#9708,#2468,.T.);
#12425=EDGE_CURVE('',#9707,#9711,#2469,.T.);
#12426=EDGE_CURVE('',#9713,#9714,#2470,.T.);
#12427=EDGE_CURVE('',#9715,#9714,#2471,.T.);
#12428=EDGE_CURVE('',#9715,#9716,#2472,.T.);
#12429=EDGE_CURVE('',#9713,#9716,#2473,.T.);
#12430=EDGE_CURVE('',#9716,#9706,#2474,.T.);
#12431=EDGE_CURVE('',#9711,#9715,#2475,.T.);
#12432=EDGE_CURVE('',#9714,#9717,#2476,.T.);
#12433=EDGE_CURVE('',#9718,#9717,#2477,.T.);
#12434=EDGE_CURVE('',#9719,#9718,#2478,.T.);
#12435=EDGE_CURVE('',#9719,#9711,#2479,.T.);
#12436=EDGE_CURVE('',#9709,#9713,#2480,.T.);
#12437=EDGE_CURVE('',#9705,#9720,#2481,.T.);
#12438=EDGE_CURVE('',#9720,#9721,#2482,.T.);
#12439=EDGE_CURVE('',#9721,#9702,#2483,.T.);
#12440=EDGE_CURVE('',#9722,#9699,#2484,.T.);
#12441=EDGE_CURVE('',#9723,#9722,#2485,.T.);
#12442=EDGE_CURVE('',#9724,#9723,#2486,.T.);
#12443=EDGE_CURVE('',#9725,#9724,#2487,.T.);
#12444=EDGE_CURVE('',#9710,#9725,#2488,.T.);
#12445=EDGE_CURVE('',#9726,#9727,#2489,.T.);
#12446=EDGE_CURVE('',#9727,#9704,#2490,.T.);
#12447=EDGE_CURVE('',#9726,#9703,#2491,.T.);
#12448=EDGE_CURVE('',#9721,#9728,#2492,.T.);
#12449=EDGE_CURVE('',#9720,#9729,#2493,.T.);
#12450=EDGE_CURVE('',#9728,#9729,#2494,.T.);
#12451=EDGE_CURVE('',#9729,#9727,#2495,.T.);
#12452=EDGE_CURVE('',#9730,#9731,#2496,.T.);
#12453=EDGE_CURVE('',#9732,#9731,#2497,.T.);
#12454=EDGE_CURVE('',#9732,#9733,#2498,.T.);
#12455=EDGE_CURVE('',#9730,#9733,#2499,.T.);
#12456=EDGE_CURVE('',#9734,#9730,#2500,.T.);
#12457=EDGE_CURVE('',#9735,#9734,#2501,.T.);
#12458=EDGE_CURVE('',#9731,#9735,#2502,.T.);
#12459=EDGE_CURVE('',#9733,#9736,#2503,.T.);
#12460=EDGE_CURVE('',#9737,#9732,#2504,.T.);
#12461=EDGE_CURVE('',#9736,#9737,#2505,.T.);
#12462=EDGE_CURVE('',#9736,#9701,#2506,.T.);
#12463=EDGE_CURVE('',#9737,#9738,#2507,.T.);
#12464=EDGE_CURVE('',#9739,#9738,#2508,.T.);
#12465=EDGE_CURVE('',#9691,#9739,#2509,.T.);
#12466=EDGE_CURVE('',#9725,#9734,#2510,.T.);
#12467=EDGE_CURVE('',#9724,#9718,#2511,.T.);
#12468=EDGE_CURVE('',#9717,#9735,#2512,.T.);
#12469=EDGE_CURVE('',#9723,#9719,#2513,.T.);
#12470=EDGE_CURVE('',#9740,#9712,#2514,.T.);
#12471=EDGE_CURVE('',#9741,#9740,#2515,.T.);
#12472=EDGE_CURVE('',#9742,#9741,#2516,.T.);
#12473=EDGE_CURVE('',#9738,#9742,#2517,.T.);
#12474=EDGE_CURVE('',#9743,#9742,#2518,.T.);
#12475=EDGE_CURVE('',#9739,#9743,#2519,.T.);
#12476=EDGE_CURVE('',#9743,#9744,#2520,.T.);
#12477=EDGE_CURVE('',#9744,#9745,#2521,.T.);
#12478=EDGE_CURVE('',#9745,#9726,#2522,.T.);
#12479=EDGE_CURVE('',#9728,#9697,#2523,.T.);
#12480=EDGE_CURVE('',#9727,#9746,#2524,.T.);
#12481=EDGE_CURVE('',#9698,#9746,#2525,.T.);
#12482=EDGE_CURVE('',#9722,#9746,#2526,.T.);
#12483=EDGE_CURVE('',#9745,#9740,#2527,.T.);
#12484=EDGE_CURVE('',#9744,#9741,#2528,.T.);
#12485=EDGE_CURVE('',#9747,#9747,#7937,.T.);
#12486=EDGE_CURVE('',#9747,#9748,#2529,.T.);
#12487=EDGE_CURVE('',#9748,#9748,#7938,.T.);
#12488=EDGE_CURVE('',#9749,#9749,#7939,.T.);
#12489=EDGE_CURVE('',#9749,#9750,#2530,.T.);
#12490=EDGE_CURVE('',#9750,#9750,#7940,.T.);
#12491=EDGE_CURVE('',#9751,#9752,#7941,.T.);
#12492=EDGE_CURVE('',#9752,#9753,#2531,.T.);
#12493=EDGE_CURVE('',#9753,#9754,#7942,.T.);
#12494=EDGE_CURVE('',#9754,#9751,#2532,.T.);
#12495=EDGE_CURVE('',#9755,#9752,#7943,.T.);
#12496=EDGE_CURVE('',#9756,#9755,#2533,.T.);
#12497=EDGE_CURVE('',#9753,#9756,#7944,.T.);
#12498=EDGE_CURVE('',#9755,#9757,#7945,.T.);
#12499=EDGE_CURVE('',#9757,#9758,#2534,.T.);
#12500=EDGE_CURVE('',#9758,#9756,#7946,.T.);
#12501=EDGE_CURVE('',#9759,#9757,#2535,.T.);
#12502=EDGE_CURVE('',#9760,#9759,#2536,.T.);
#12503=EDGE_CURVE('',#9758,#9760,#2537,.T.);
#12504=EDGE_CURVE('',#9761,#9762,#7947,.T.);
#12505=EDGE_CURVE('',#9762,#9763,#2538,.T.);
#12506=EDGE_CURVE('',#9763,#9764,#7948,.T.);
#12507=EDGE_CURVE('',#9764,#9761,#2539,.T.);
#12508=EDGE_CURVE('',#9765,#9762,#7949,.T.);
#12509=EDGE_CURVE('',#9766,#9765,#2540,.T.);
#12510=EDGE_CURVE('',#9763,#9766,#7950,.T.);
#12511=EDGE_CURVE('',#9765,#9767,#7951,.T.);
#12512=EDGE_CURVE('',#9767,#9768,#2541,.T.);
#12513=EDGE_CURVE('',#9768,#9766,#7952,.T.);
#12514=EDGE_CURVE('',#9769,#9767,#2542,.T.);
#12515=EDGE_CURVE('',#9770,#9769,#2543,.T.);
#12516=EDGE_CURVE('',#9768,#9770,#2544,.T.);
#12517=EDGE_CURVE('',#9771,#9772,#7953,.T.);
#12518=EDGE_CURVE('',#9772,#9773,#2545,.T.);
#12519=EDGE_CURVE('',#9773,#9774,#7954,.T.);
#12520=EDGE_CURVE('',#9774,#9771,#2546,.T.);
#12521=EDGE_CURVE('',#9775,#9772,#7955,.T.);
#12522=EDGE_CURVE('',#9776,#9775,#2547,.T.);
#12523=EDGE_CURVE('',#9773,#9776,#7956,.T.);
#12524=EDGE_CURVE('',#9775,#9777,#7957,.T.);
#12525=EDGE_CURVE('',#9777,#9778,#2548,.T.);
#12526=EDGE_CURVE('',#9778,#9776,#7958,.T.);
#12527=EDGE_CURVE('',#9779,#9777,#2549,.T.);
#12528=EDGE_CURVE('',#9780,#9779,#2550,.T.);
#12529=EDGE_CURVE('',#9778,#9780,#2551,.T.);
#12530=EDGE_CURVE('',#9781,#9782,#7959,.T.);
#12531=EDGE_CURVE('',#9782,#9783,#2552,.T.);
#12532=EDGE_CURVE('',#9783,#9784,#7960,.T.);
#12533=EDGE_CURVE('',#9784,#9781,#2553,.T.);
#12534=EDGE_CURVE('',#9785,#9782,#7961,.T.);
#12535=EDGE_CURVE('',#9786,#9785,#2554,.T.);
#12536=EDGE_CURVE('',#9783,#9786,#7962,.T.);
#12537=EDGE_CURVE('',#9785,#9787,#7963,.T.);
#12538=EDGE_CURVE('',#9787,#9788,#2555,.T.);
#12539=EDGE_CURVE('',#9788,#9786,#7964,.T.);
#12540=EDGE_CURVE('',#9789,#9787,#2556,.T.);
#12541=EDGE_CURVE('',#9790,#9789,#2557,.T.);
#12542=EDGE_CURVE('',#9788,#9790,#2558,.T.);
#12543=EDGE_CURVE('',#9791,#9792,#7965,.T.);
#12544=EDGE_CURVE('',#9792,#9793,#2559,.T.);
#12545=EDGE_CURVE('',#9793,#9794,#7966,.T.);
#12546=EDGE_CURVE('',#9794,#9791,#2560,.T.);
#12547=EDGE_CURVE('',#9795,#9792,#7967,.T.);
#12548=EDGE_CURVE('',#9796,#9795,#2561,.T.);
#12549=EDGE_CURVE('',#9793,#9796,#7968,.T.);
#12550=EDGE_CURVE('',#9795,#9797,#7969,.T.);
#12551=EDGE_CURVE('',#9797,#9798,#2562,.T.);
#12552=EDGE_CURVE('',#9798,#9796,#7970,.T.);
#12553=EDGE_CURVE('',#9799,#9797,#2563,.T.);
#12554=EDGE_CURVE('',#9800,#9799,#2564,.T.);
#12555=EDGE_CURVE('',#9798,#9800,#2565,.T.);
#12556=EDGE_CURVE('',#9801,#9794,#2566,.T.);
#12557=EDGE_CURVE('',#9802,#9801,#2567,.T.);
#12558=EDGE_CURVE('',#9791,#9802,#2568,.T.);
#12559=EDGE_CURVE('',#9803,#9784,#2569,.T.);
#12560=EDGE_CURVE('',#9804,#9803,#2570,.T.);
#12561=EDGE_CURVE('',#9781,#9804,#2571,.T.);
#12562=EDGE_CURVE('',#9805,#9764,#2572,.T.);
#12563=EDGE_CURVE('',#9806,#9805,#2573,.T.);
#12564=EDGE_CURVE('',#9761,#9806,#2574,.T.);
#12565=EDGE_CURVE('',#9807,#9754,#2575,.T.);
#12566=EDGE_CURVE('',#9808,#9807,#2576,.T.);
#12567=EDGE_CURVE('',#9751,#9808,#2577,.T.);
#12568=EDGE_CURVE('',#9809,#9799,#7971,.T.);
#12569=EDGE_CURVE('',#9809,#9810,#2578,.T.);
#12570=EDGE_CURVE('',#9800,#9810,#7972,.T.);
#12571=EDGE_CURVE('',#9780,#9803,#7973,.T.);
#12572=EDGE_CURVE('',#9804,#9779,#7974,.T.);
#12573=EDGE_CURVE('',#9810,#9811,#2579,.T.);
#12574=EDGE_CURVE('',#9811,#9812,#7975,.T.);
#12575=EDGE_CURVE('',#9812,#9813,#2580,.T.);
#12576=EDGE_CURVE('',#9813,#9807,#7976,.T.);
#12577=EDGE_CURVE('',#9760,#9805,#7977,.T.);
#12578=EDGE_CURVE('',#9770,#9814,#7978,.T.);
#12579=EDGE_CURVE('',#9814,#9774,#2581,.T.);
#12580=EDGE_CURVE('',#9790,#9801,#7979,.T.);
#12581=EDGE_CURVE('',#9815,#9769,#7980,.T.);
#12582=EDGE_CURVE('',#9815,#9814,#2582,.T.);
#12583=EDGE_CURVE('',#9813,#9816,#2583,.T.);
#12584=EDGE_CURVE('',#9808,#9816,#7981,.T.);
#12585=EDGE_CURVE('',#9771,#9815,#2584,.T.);
#12586=EDGE_CURVE('',#9802,#9789,#7982,.T.);
#12587=EDGE_CURVE('',#9817,#9809,#2585,.T.);
#12588=EDGE_CURVE('',#9811,#9817,#2586,.T.);
#12589=EDGE_CURVE('',#9818,#9817,#7983,.T.);
#12590=EDGE_CURVE('',#9812,#9818,#2587,.T.);
#12591=EDGE_CURVE('',#9816,#9818,#2588,.T.);
#12592=EDGE_CURVE('',#9806,#9759,#7984,.T.);
#12593=EDGE_CURVE('',#9819,#9820,#7985,.T.);
#12594=EDGE_CURVE('',#9820,#9821,#2589,.T.);
#12595=EDGE_CURVE('',#9821,#9822,#7986,.T.);
#12596=EDGE_CURVE('',#9822,#9819,#2590,.T.);
#12597=EDGE_CURVE('',#9823,#9820,#7987,.T.);
#12598=EDGE_CURVE('',#9824,#9823,#2591,.T.);
#12599=EDGE_CURVE('',#9821,#9824,#7988,.T.);
#12600=EDGE_CURVE('',#9823,#9825,#7989,.T.);
#12601=EDGE_CURVE('',#9825,#9826,#2592,.T.);
#12602=EDGE_CURVE('',#9826,#9824,#7990,.T.);
#12603=EDGE_CURVE('',#9827,#9825,#2593,.T.);
#12604=EDGE_CURVE('',#9828,#9827,#2594,.T.);
#12605=EDGE_CURVE('',#9826,#9828,#2595,.T.);
#12606=EDGE_CURVE('',#9829,#9830,#7991,.T.);
#12607=EDGE_CURVE('',#9830,#9831,#2596,.T.);
#12608=EDGE_CURVE('',#9831,#9832,#7992,.T.);
#12609=EDGE_CURVE('',#9832,#9829,#2597,.T.);
#12610=EDGE_CURVE('',#9833,#9830,#7993,.T.);
#12611=EDGE_CURVE('',#9834,#9833,#2598,.T.);
#12612=EDGE_CURVE('',#9831,#9834,#7994,.T.);
#12613=EDGE_CURVE('',#9833,#9835,#7995,.T.);
#12614=EDGE_CURVE('',#9835,#9836,#2599,.T.);
#12615=EDGE_CURVE('',#9836,#9834,#7996,.T.);
#12616=EDGE_CURVE('',#9837,#9835,#2600,.T.);
#12617=EDGE_CURVE('',#9838,#9837,#2601,.T.);
#12618=EDGE_CURVE('',#9836,#9838,#2602,.T.);
#12619=EDGE_CURVE('',#9839,#9840,#7997,.T.);
#12620=EDGE_CURVE('',#9840,#9841,#2603,.T.);
#12621=EDGE_CURVE('',#9841,#9842,#7998,.T.);
#12622=EDGE_CURVE('',#9842,#9839,#2604,.T.);
#12623=EDGE_CURVE('',#9843,#9840,#7999,.T.);
#12624=EDGE_CURVE('',#9844,#9843,#2605,.T.);
#12625=EDGE_CURVE('',#9841,#9844,#8000,.T.);
#12626=EDGE_CURVE('',#9843,#9845,#8001,.T.);
#12627=EDGE_CURVE('',#9845,#9846,#2606,.T.);
#12628=EDGE_CURVE('',#9846,#9844,#8002,.T.);
#12629=EDGE_CURVE('',#9847,#9845,#2607,.T.);
#12630=EDGE_CURVE('',#9848,#9847,#2608,.T.);
#12631=EDGE_CURVE('',#9846,#9848,#2609,.T.);
#12632=EDGE_CURVE('',#9849,#9850,#8003,.T.);
#12633=EDGE_CURVE('',#9850,#9851,#2610,.T.);
#12634=EDGE_CURVE('',#9851,#9852,#8004,.T.);
#12635=EDGE_CURVE('',#9852,#9849,#2611,.T.);
#12636=EDGE_CURVE('',#9853,#9850,#8005,.T.);
#12637=EDGE_CURVE('',#9854,#9853,#2612,.T.);
#12638=EDGE_CURVE('',#9851,#9854,#8006,.T.);
#12639=EDGE_CURVE('',#9853,#9855,#8007,.T.);
#12640=EDGE_CURVE('',#9855,#9856,#2613,.T.);
#12641=EDGE_CURVE('',#9856,#9854,#8008,.T.);
#12642=EDGE_CURVE('',#9857,#9855,#2614,.T.);
#12643=EDGE_CURVE('',#9858,#9857,#2615,.T.);
#12644=EDGE_CURVE('',#9856,#9858,#2616,.T.);
#12645=EDGE_CURVE('',#9859,#9860,#8009,.T.);
#12646=EDGE_CURVE('',#9860,#9861,#2617,.T.);
#12647=EDGE_CURVE('',#9861,#9862,#8010,.T.);
#12648=EDGE_CURVE('',#9862,#9859,#2618,.T.);
#12649=EDGE_CURVE('',#9863,#9860,#8011,.T.);
#12650=EDGE_CURVE('',#9864,#9863,#2619,.T.);
#12651=EDGE_CURVE('',#9861,#9864,#8012,.T.);
#12652=EDGE_CURVE('',#9863,#9865,#8013,.T.);
#12653=EDGE_CURVE('',#9865,#9866,#2620,.T.);
#12654=EDGE_CURVE('',#9866,#9864,#8014,.T.);
#12655=EDGE_CURVE('',#9867,#9865,#2621,.T.);
#12656=EDGE_CURVE('',#9868,#9867,#2622,.T.);
#12657=EDGE_CURVE('',#9866,#9868,#2623,.T.);
#12658=EDGE_CURVE('',#9869,#9862,#2624,.T.);
#12659=EDGE_CURVE('',#9870,#9869,#2625,.T.);
#12660=EDGE_CURVE('',#9859,#9870,#2626,.T.);
#12661=EDGE_CURVE('',#9871,#9852,#2627,.T.);
#12662=EDGE_CURVE('',#9872,#9871,#2628,.T.);
#12663=EDGE_CURVE('',#9849,#9872,#2629,.T.);
#12664=EDGE_CURVE('',#9873,#9832,#2630,.T.);
#12665=EDGE_CURVE('',#9874,#9873,#2631,.T.);
#12666=EDGE_CURVE('',#9829,#9874,#2632,.T.);
#12667=EDGE_CURVE('',#9875,#9822,#2633,.T.);
#12668=EDGE_CURVE('',#9876,#9875,#2634,.T.);
#12669=EDGE_CURVE('',#9819,#9876,#2635,.T.);
#12670=EDGE_CURVE('',#9877,#9867,#8015,.T.);
#12671=EDGE_CURVE('',#9877,#9878,#2636,.T.);
#12672=EDGE_CURVE('',#9868,#9878,#8016,.T.);
#12673=EDGE_CURVE('',#9848,#9871,#8017,.T.);
#12674=EDGE_CURVE('',#9872,#9847,#8018,.T.);
#12675=EDGE_CURVE('',#9878,#9879,#2637,.T.);
#12676=EDGE_CURVE('',#9879,#9880,#8019,.T.);
#12677=EDGE_CURVE('',#9880,#9881,#2638,.T.);
#12678=EDGE_CURVE('',#9881,#9875,#8020,.T.);
#12679=EDGE_CURVE('',#9828,#9873,#8021,.T.);
#12680=EDGE_CURVE('',#9838,#9882,#8022,.T.);
#12681=EDGE_CURVE('',#9882,#9842,#2639,.T.);
#12682=EDGE_CURVE('',#9858,#9869,#8023,.T.);
#12683=EDGE_CURVE('',#9883,#9837,#8024,.T.);
#12684=EDGE_CURVE('',#9883,#9882,#2640,.T.);
#12685=EDGE_CURVE('',#9881,#9884,#2641,.T.);
#12686=EDGE_CURVE('',#9876,#9884,#8025,.T.);
#12687=EDGE_CURVE('',#9839,#9883,#2642,.T.);
#12688=EDGE_CURVE('',#9870,#9857,#8026,.T.);
#12689=EDGE_CURVE('',#9885,#9877,#2643,.T.);
#12690=EDGE_CURVE('',#9879,#9885,#2644,.T.);
#12691=EDGE_CURVE('',#9886,#9885,#8027,.T.);
#12692=EDGE_CURVE('',#9880,#9886,#2645,.T.);
#12693=EDGE_CURVE('',#9884,#9886,#2646,.T.);
#12694=EDGE_CURVE('',#9874,#9827,#8028,.T.);
#12695=EDGE_CURVE('',#9887,#9888,#8029,.T.);
#12696=EDGE_CURVE('',#9888,#9889,#8030,.T.);
#12697=EDGE_CURVE('',#9889,#9889,#8031,.T.);
#12698=EDGE_CURVE('',#9888,#9887,#8032,.T.);
#12699=EDGE_CURVE('',#9890,#9891,#8033,.T.);
#12700=EDGE_CURVE('',#9890,#9887,#2647,.T.);
#12701=EDGE_CURVE('',#9891,#9890,#8034,.T.);
#12702=EDGE_CURVE('',#9892,#9892,#8035,.T.);
#12703=EDGE_CURVE('',#9893,#9893,#8036,.T.);
#12704=EDGE_CURVE('',#9893,#9891,#8037,.T.);
#12705=EDGE_CURVE('',#9894,#9894,#8038,.T.);
#12706=EDGE_CURVE('',#9892,#9894,#2648,.T.);
#12707=EDGE_CURVE('',#9895,#9896,#2649,.T.);
#12708=EDGE_CURVE('',#9896,#9897,#2650,.T.);
#12709=EDGE_CURVE('',#9897,#9898,#2651,.T.);
#12710=EDGE_CURVE('',#9895,#9898,#2652,.T.);
#12711=EDGE_CURVE('',#9899,#9900,#2653,.T.);
#12712=EDGE_CURVE('',#9899,#9901,#2654,.T.);
#12713=EDGE_CURVE('',#9901,#9902,#2655,.T.);
#12714=EDGE_CURVE('',#9900,#9902,#2656,.T.);
#12715=EDGE_CURVE('',#9903,#9904,#2657,.T.);
#12716=EDGE_CURVE('',#9903,#9899,#8039,.T.);
#12717=EDGE_CURVE('',#9904,#9900,#8040,.T.);
#12718=EDGE_CURVE('',#9902,#9897,#2658,.T.);
#12719=EDGE_CURVE('',#9898,#9901,#2659,.T.);
#12720=EDGE_CURVE('',#9905,#9896,#2660,.T.);
#12721=EDGE_CURVE('',#9906,#9905,#2661,.T.);
#12722=EDGE_CURVE('',#9904,#9906,#2662,.T.);
#12723=EDGE_CURVE('',#9907,#9906,#2663,.T.);
#12724=EDGE_CURVE('',#9903,#9907,#2664,.T.);
#12725=EDGE_CURVE('',#9908,#9907,#2665,.T.);
#12726=EDGE_CURVE('',#9895,#9908,#2666,.T.);
#12727=EDGE_CURVE('',#9905,#9908,#2667,.T.);
#12728=EDGE_CURVE('',#9909,#9910,#8041,.T.);
#12729=EDGE_CURVE('',#9910,#9911,#2668,.T.);
#12730=EDGE_CURVE('',#9911,#9911,#8042,.T.);
#12731=EDGE_CURVE('',#9910,#9909,#8043,.T.);
#12732=EDGE_CURVE('',#9909,#9912,#2669,.T.);
#12733=EDGE_CURVE('',#9912,#9912,#8044,.T.);
#12734=EDGE_CURVE('',#9913,#9914,#220,.F.);
#12735=EDGE_CURVE('',#9914,#9915,#8045,.T.);
#12736=EDGE_CURVE('',#9915,#9916,#221,.F.);
#12737=EDGE_CURVE('',#9916,#9913,#8046,.T.);
#12738=EDGE_CURVE('',#9914,#9917,#158,.T.);
#12739=EDGE_CURVE('',#9917,#9918,#8047,.T.);
#12740=EDGE_CURVE('',#9918,#9915,#159,.T.);
#12741=EDGE_CURVE('',#9919,#9920,#222,.F.);
#12742=EDGE_CURVE('',#9920,#9921,#8048,.T.);
#12743=EDGE_CURVE('',#9921,#9922,#223,.F.);
#12744=EDGE_CURVE('',#9922,#9919,#8049,.T.);
#12745=EDGE_CURVE('',#9920,#9923,#160,.T.);
#12746=EDGE_CURVE('',#9923,#9924,#8050,.T.);
#12747=EDGE_CURVE('',#9924,#9921,#161,.T.);
#12748=EDGE_CURVE('',#9925,#9926,#224,.F.);
#12749=EDGE_CURVE('',#9926,#9927,#8051,.T.);
#12750=EDGE_CURVE('',#9927,#9928,#225,.F.);
#12751=EDGE_CURVE('',#9928,#9925,#8052,.T.);
#12752=EDGE_CURVE('',#9926,#9929,#162,.T.);
#12753=EDGE_CURVE('',#9929,#9930,#8053,.T.);
#12754=EDGE_CURVE('',#9930,#9931,#8054,.T.);
#12755=EDGE_CURVE('',#9931,#9927,#163,.T.);
#12756=EDGE_CURVE('',#9932,#9933,#226,.F.);
#12757=EDGE_CURVE('',#9933,#9934,#8055,.T.);
#12758=EDGE_CURVE('',#9934,#9935,#227,.F.);
#12759=EDGE_CURVE('',#9935,#9932,#8056,.T.);
#12760=EDGE_CURVE('',#9933,#9936,#164,.T.);
#12761=EDGE_CURVE('',#9936,#9937,#8057,.T.);
#12762=EDGE_CURVE('',#9937,#9934,#165,.T.);
#12763=EDGE_CURVE('',#9938,#9939,#8058,.T.);
#12764=EDGE_CURVE('',#9939,#9940,#8059,.T.);
#12765=EDGE_CURVE('',#9940,#9940,#8060,.T.);
#12766=EDGE_CURVE('',#9939,#9938,#8061,.T.);
#12767=EDGE_CURVE('',#9941,#9916,#8062,.T.);
#12768=EDGE_CURVE('',#9942,#9941,#228,.F.);
#12769=EDGE_CURVE('',#9932,#9942,#8063,.T.);
#12770=EDGE_CURVE('',#9943,#9935,#8064,.T.);
#12771=EDGE_CURVE('',#9944,#9943,#229,.F.);
#12772=EDGE_CURVE('',#9925,#9944,#8065,.T.);
#12773=EDGE_CURVE('',#9945,#9928,#8066,.T.);
#12774=EDGE_CURVE('',#9946,#9945,#230,.F.);
#12775=EDGE_CURVE('',#9919,#9946,#8067,.T.);
#12776=EDGE_CURVE('',#9947,#9922,#8068,.T.);
#12777=EDGE_CURVE('',#9948,#9947,#231,.F.);
#12778=EDGE_CURVE('',#9913,#9948,#8069,.T.);
#12779=EDGE_CURVE('',#9949,#9949,#8070,.T.);
#12780=EDGE_CURVE('',#9949,#9938,#2670,.T.);
#12781=EDGE_CURVE('',#9941,#9950,#2671,.T.);
#12782=EDGE_CURVE('',#9951,#9950,#232,.F.);
#12783=EDGE_CURVE('',#9942,#9951,#2672,.T.);
#12784=EDGE_CURVE('',#9950,#9918,#166,.T.);
#12785=EDGE_CURVE('',#9948,#9952,#2673,.T.);
#12786=EDGE_CURVE('',#9917,#9952,#167,.T.);
#12787=EDGE_CURVE('',#9947,#9953,#2674,.T.);
#12788=EDGE_CURVE('',#9952,#9953,#233,.F.);
#12789=EDGE_CURVE('',#9954,#9931,#168,.T.);
#12790=EDGE_CURVE('',#9945,#9954,#2675,.T.);
#12791=EDGE_CURVE('',#9953,#9924,#169,.T.);
#12792=EDGE_CURVE('',#9936,#9951,#170,.T.);
#12793=EDGE_CURVE('',#9955,#9937,#171,.T.);
#12794=EDGE_CURVE('',#9943,#9955,#2676,.T.);
#12795=EDGE_CURVE('',#9946,#9956,#2677,.T.);
#12796=EDGE_CURVE('',#9923,#9956,#172,.T.);
#12797=EDGE_CURVE('',#9956,#9954,#234,.F.);
#12798=EDGE_CURVE('',#9957,#9955,#235,.F.);
#12799=EDGE_CURVE('',#9944,#9957,#2678,.T.);
#12800=EDGE_CURVE('',#9929,#9957,#173,.T.);
#12801=EDGE_CURVE('',#9958,#9930,#2679,.T.);
#12802=EDGE_CURVE('',#9959,#9959,#8071,.T.);
#12803=EDGE_CURVE('',#9959,#9960,#2680,.T.);
#12804=EDGE_CURVE('',#9960,#9960,#8072,.T.);
#12805=EDGE_CURVE('',#9912,#9959,#2681,.T.);
#12806=ORIENTED_EDGE('',*,*,#9961,.T.);
#12807=ORIENTED_EDGE('',*,*,#9962,.T.);
#12808=ORIENTED_EDGE('',*,*,#9963,.T.);
#12809=ORIENTED_EDGE('',*,*,#9964,.T.);
#12810=ORIENTED_EDGE('',*,*,#9962,.F.);
#12811=ORIENTED_EDGE('',*,*,#9964,.F.);
#12812=ORIENTED_EDGE('',*,*,#9965,.T.);
#12813=ORIENTED_EDGE('',*,*,#9966,.F.);
#12814=ORIENTED_EDGE('',*,*,#9967,.F.);
#12815=ORIENTED_EDGE('',*,*,#9965,.F.);
#12816=ORIENTED_EDGE('',*,*,#9963,.F.);
#12817=ORIENTED_EDGE('',*,*,#9961,.F.);
#12818=ORIENTED_EDGE('',*,*,#9968,.F.);
#12819=ORIENTED_EDGE('',*,*,#9967,.T.);
#12820=ORIENTED_EDGE('',*,*,#9969,.T.);
#12821=ORIENTED_EDGE('',*,*,#9970,.T.);
#12822=ORIENTED_EDGE('',*,*,#9969,.F.);
#12823=ORIENTED_EDGE('',*,*,#9966,.T.);
#12824=ORIENTED_EDGE('',*,*,#9970,.F.);
#12825=ORIENTED_EDGE('',*,*,#9971,.T.);
#12826=ORIENTED_EDGE('',*,*,#9971,.F.);
#12827=ORIENTED_EDGE('',*,*,#9972,.T.);
#12828=ORIENTED_EDGE('',*,*,#9968,.T.);
#12829=ORIENTED_EDGE('',*,*,#9972,.F.);
#12830=ORIENTED_EDGE('',*,*,#9973,.T.);
#12831=ORIENTED_EDGE('',*,*,#9974,.T.);
#12832=ORIENTED_EDGE('',*,*,#9975,.T.);
#12833=ORIENTED_EDGE('',*,*,#9976,.T.);
#12834=ORIENTED_EDGE('',*,*,#9974,.F.);
#12835=ORIENTED_EDGE('',*,*,#9977,.F.);
#12836=ORIENTED_EDGE('',*,*,#9978,.F.);
#12837=ORIENTED_EDGE('',*,*,#9979,.F.);
#12838=ORIENTED_EDGE('',*,*,#9980,.T.);
#12839=ORIENTED_EDGE('',*,*,#9981,.T.);
#12840=ORIENTED_EDGE('',*,*,#9982,.T.);
#12841=ORIENTED_EDGE('',*,*,#9978,.T.);
#12842=ORIENTED_EDGE('',*,*,#9981,.F.);
#12843=ORIENTED_EDGE('',*,*,#9983,.F.);
#12844=ORIENTED_EDGE('',*,*,#9984,.F.);
#12845=ORIENTED_EDGE('',*,*,#9985,.F.);
#12846=ORIENTED_EDGE('',*,*,#9986,.T.);
#12847=ORIENTED_EDGE('',*,*,#9987,.T.);
#12848=ORIENTED_EDGE('',*,*,#9988,.T.);
#12849=ORIENTED_EDGE('',*,*,#9989,.T.);
#12850=ORIENTED_EDGE('',*,*,#9987,.F.);
#12851=ORIENTED_EDGE('',*,*,#9990,.F.);
#12852=ORIENTED_EDGE('',*,*,#9991,.F.);
#12853=ORIENTED_EDGE('',*,*,#9992,.F.);
#12854=ORIENTED_EDGE('',*,*,#9993,.T.);
#12855=ORIENTED_EDGE('',*,*,#9994,.T.);
#12856=ORIENTED_EDGE('',*,*,#9995,.T.);
#12857=ORIENTED_EDGE('',*,*,#9991,.T.);
#12858=ORIENTED_EDGE('',*,*,#9994,.F.);
#12859=ORIENTED_EDGE('',*,*,#9996,.F.);
#12860=ORIENTED_EDGE('',*,*,#9997,.F.);
#12861=ORIENTED_EDGE('',*,*,#9998,.F.);
#12862=ORIENTED_EDGE('',*,*,#9999,.T.);
#12863=ORIENTED_EDGE('',*,*,#10000,.T.);
#12864=ORIENTED_EDGE('',*,*,#10001,.T.);
#12865=ORIENTED_EDGE('',*,*,#10002,.T.);
#12866=ORIENTED_EDGE('',*,*,#10000,.F.);
#12867=ORIENTED_EDGE('',*,*,#10003,.F.);
#12868=ORIENTED_EDGE('',*,*,#10004,.F.);
#12869=ORIENTED_EDGE('',*,*,#10005,.F.);
#12870=ORIENTED_EDGE('',*,*,#10006,.T.);
#12871=ORIENTED_EDGE('',*,*,#10007,.T.);
#12872=ORIENTED_EDGE('',*,*,#10008,.T.);
#12873=ORIENTED_EDGE('',*,*,#10004,.T.);
#12874=ORIENTED_EDGE('',*,*,#10007,.F.);
#12875=ORIENTED_EDGE('',*,*,#10009,.F.);
#12876=ORIENTED_EDGE('',*,*,#10010,.F.);
#12877=ORIENTED_EDGE('',*,*,#10011,.F.);
#12878=ORIENTED_EDGE('',*,*,#10012,.T.);
#12879=ORIENTED_EDGE('',*,*,#10013,.T.);
#12880=ORIENTED_EDGE('',*,*,#10014,.T.);
#12881=ORIENTED_EDGE('',*,*,#10015,.T.);
#12882=ORIENTED_EDGE('',*,*,#10013,.F.);
#12883=ORIENTED_EDGE('',*,*,#10016,.F.);
#12884=ORIENTED_EDGE('',*,*,#10017,.F.);
#12885=ORIENTED_EDGE('',*,*,#10018,.F.);
#12886=ORIENTED_EDGE('',*,*,#10019,.T.);
#12887=ORIENTED_EDGE('',*,*,#10020,.T.);
#12888=ORIENTED_EDGE('',*,*,#10021,.T.);
#12889=ORIENTED_EDGE('',*,*,#10017,.T.);
#12890=ORIENTED_EDGE('',*,*,#10020,.F.);
#12891=ORIENTED_EDGE('',*,*,#10022,.F.);
#12892=ORIENTED_EDGE('',*,*,#10023,.F.);
#12893=ORIENTED_EDGE('',*,*,#10024,.F.);
#12894=ORIENTED_EDGE('',*,*,#10025,.T.);
#12895=ORIENTED_EDGE('',*,*,#10026,.T.);
#12896=ORIENTED_EDGE('',*,*,#10027,.T.);
#12897=ORIENTED_EDGE('',*,*,#10028,.T.);
#12898=ORIENTED_EDGE('',*,*,#10026,.F.);
#12899=ORIENTED_EDGE('',*,*,#10029,.F.);
#12900=ORIENTED_EDGE('',*,*,#10030,.F.);
#12901=ORIENTED_EDGE('',*,*,#10031,.F.);
#12902=ORIENTED_EDGE('',*,*,#10032,.T.);
#12903=ORIENTED_EDGE('',*,*,#10033,.T.);
#12904=ORIENTED_EDGE('',*,*,#10034,.T.);
#12905=ORIENTED_EDGE('',*,*,#10030,.T.);
#12906=ORIENTED_EDGE('',*,*,#10033,.F.);
#12907=ORIENTED_EDGE('',*,*,#10035,.F.);
#12908=ORIENTED_EDGE('',*,*,#10036,.F.);
#12909=ORIENTED_EDGE('',*,*,#10037,.F.);
#12910=ORIENTED_EDGE('',*,*,#10028,.F.);
#12911=ORIENTED_EDGE('',*,*,#10038,.F.);
#12912=ORIENTED_EDGE('',*,*,#10039,.F.);
#12913=ORIENTED_EDGE('',*,*,#10040,.F.);
#12914=ORIENTED_EDGE('',*,*,#10015,.F.);
#12915=ORIENTED_EDGE('',*,*,#10041,.F.);
#12916=ORIENTED_EDGE('',*,*,#10042,.F.);
#12917=ORIENTED_EDGE('',*,*,#10043,.F.);
#12918=ORIENTED_EDGE('',*,*,#9989,.F.);
#12919=ORIENTED_EDGE('',*,*,#10044,.F.);
#12920=ORIENTED_EDGE('',*,*,#10045,.F.);
#12921=ORIENTED_EDGE('',*,*,#10046,.F.);
#12922=ORIENTED_EDGE('',*,*,#9976,.F.);
#12923=ORIENTED_EDGE('',*,*,#10047,.F.);
#12924=ORIENTED_EDGE('',*,*,#10048,.F.);
#12925=ORIENTED_EDGE('',*,*,#10049,.F.);
#12926=ORIENTED_EDGE('',*,*,#10036,.T.);
#12927=ORIENTED_EDGE('',*,*,#10050,.F.);
#12928=ORIENTED_EDGE('',*,*,#10051,.F.);
#12929=ORIENTED_EDGE('',*,*,#10052,.F.);
#12930=ORIENTED_EDGE('',*,*,#10042,.T.);
#12931=ORIENTED_EDGE('',*,*,#10053,.F.);
#12932=ORIENTED_EDGE('',*,*,#10010,.T.);
#12933=ORIENTED_EDGE('',*,*,#10054,.F.);
#12934=ORIENTED_EDGE('',*,*,#10038,.T.);
#12935=ORIENTED_EDGE('',*,*,#10027,.F.);
#12936=ORIENTED_EDGE('',*,*,#10031,.T.);
#12937=ORIENTED_EDGE('',*,*,#10034,.F.);
#12938=ORIENTED_EDGE('',*,*,#10037,.T.);
#12939=ORIENTED_EDGE('',*,*,#10052,.T.);
#12940=ORIENTED_EDGE('',*,*,#10055,.T.);
#12941=ORIENTED_EDGE('',*,*,#10056,.T.);
#12942=ORIENTED_EDGE('',*,*,#10057,.T.);
#12943=ORIENTED_EDGE('',*,*,#10058,.T.);
#12944=ORIENTED_EDGE('',*,*,#10047,.T.);
#12945=ORIENTED_EDGE('',*,*,#9975,.F.);
#12946=ORIENTED_EDGE('',*,*,#9979,.T.);
#12947=ORIENTED_EDGE('',*,*,#9982,.F.);
#12948=ORIENTED_EDGE('',*,*,#9985,.T.);
#12949=ORIENTED_EDGE('',*,*,#10059,.T.);
#12950=ORIENTED_EDGE('',*,*,#10044,.T.);
#12951=ORIENTED_EDGE('',*,*,#9988,.F.);
#12952=ORIENTED_EDGE('',*,*,#9992,.T.);
#12953=ORIENTED_EDGE('',*,*,#9995,.F.);
#12954=ORIENTED_EDGE('',*,*,#9998,.T.);
#12955=ORIENTED_EDGE('',*,*,#10060,.T.);
#12956=ORIENTED_EDGE('',*,*,#10061,.T.);
#12957=ORIENTED_EDGE('',*,*,#10001,.F.);
#12958=ORIENTED_EDGE('',*,*,#10005,.T.);
#12959=ORIENTED_EDGE('',*,*,#10008,.F.);
#12960=ORIENTED_EDGE('',*,*,#10011,.T.);
#12961=ORIENTED_EDGE('',*,*,#10053,.T.);
#12962=ORIENTED_EDGE('',*,*,#10041,.T.);
#12963=ORIENTED_EDGE('',*,*,#10014,.F.);
#12964=ORIENTED_EDGE('',*,*,#10018,.T.);
#12965=ORIENTED_EDGE('',*,*,#10021,.F.);
#12966=ORIENTED_EDGE('',*,*,#10024,.T.);
#12967=ORIENTED_EDGE('',*,*,#10062,.T.);
#12968=ORIENTED_EDGE('',*,*,#9997,.T.);
#12969=ORIENTED_EDGE('',*,*,#10063,.F.);
#12970=ORIENTED_EDGE('',*,*,#10064,.T.);
#12971=ORIENTED_EDGE('',*,*,#10060,.F.);
#12972=ORIENTED_EDGE('',*,*,#10048,.T.);
#12973=ORIENTED_EDGE('',*,*,#10058,.F.);
#12974=ORIENTED_EDGE('',*,*,#10065,.T.);
#12975=ORIENTED_EDGE('',*,*,#10066,.F.);
#12976=ORIENTED_EDGE('',*,*,#10002,.F.);
#12977=ORIENTED_EDGE('',*,*,#10061,.F.);
#12978=ORIENTED_EDGE('',*,*,#10064,.F.);
#12979=ORIENTED_EDGE('',*,*,#10067,.F.);
#12980=ORIENTED_EDGE('',*,*,#10039,.T.);
#12981=ORIENTED_EDGE('',*,*,#10062,.F.);
#12982=ORIENTED_EDGE('',*,*,#10023,.T.);
#12983=ORIENTED_EDGE('',*,*,#10068,.F.);
#12984=ORIENTED_EDGE('',*,*,#10069,.F.);
#12985=ORIENTED_EDGE('',*,*,#10070,.F.);
#12986=ORIENTED_EDGE('',*,*,#10071,.F.);
#12987=ORIENTED_EDGE('',*,*,#10056,.F.);
#12988=ORIENTED_EDGE('',*,*,#10071,.T.);
#12989=ORIENTED_EDGE('',*,*,#10072,.F.);
#12990=ORIENTED_EDGE('',*,*,#10065,.F.);
#12991=ORIENTED_EDGE('',*,*,#10057,.F.);
#12992=ORIENTED_EDGE('',*,*,#10045,.T.);
#12993=ORIENTED_EDGE('',*,*,#10059,.F.);
#12994=ORIENTED_EDGE('',*,*,#9984,.T.);
#12995=ORIENTED_EDGE('',*,*,#10073,.F.);
#12996=ORIENTED_EDGE('',*,*,#10051,.T.);
#12997=ORIENTED_EDGE('',*,*,#10074,.F.);
#12998=ORIENTED_EDGE('',*,*,#10069,.T.);
#12999=ORIENTED_EDGE('',*,*,#10055,.F.);
#13000=ORIENTED_EDGE('',*,*,#10040,.T.);
#13001=ORIENTED_EDGE('',*,*,#10068,.T.);
#13002=ORIENTED_EDGE('',*,*,#10022,.T.);
#13003=ORIENTED_EDGE('',*,*,#10019,.F.);
#13004=ORIENTED_EDGE('',*,*,#10016,.T.);
#13005=ORIENTED_EDGE('',*,*,#10012,.F.);
#13006=ORIENTED_EDGE('',*,*,#10043,.T.);
#13007=ORIENTED_EDGE('',*,*,#10054,.T.);
#13008=ORIENTED_EDGE('',*,*,#10009,.T.);
#13009=ORIENTED_EDGE('',*,*,#10006,.F.);
#13010=ORIENTED_EDGE('',*,*,#10003,.T.);
#13011=ORIENTED_EDGE('',*,*,#9999,.F.);
#13012=ORIENTED_EDGE('',*,*,#10067,.T.);
#13013=ORIENTED_EDGE('',*,*,#10063,.T.);
#13014=ORIENTED_EDGE('',*,*,#9996,.T.);
#13015=ORIENTED_EDGE('',*,*,#9993,.F.);
#13016=ORIENTED_EDGE('',*,*,#9990,.T.);
#13017=ORIENTED_EDGE('',*,*,#9986,.F.);
#13018=ORIENTED_EDGE('',*,*,#10046,.T.);
#13019=ORIENTED_EDGE('',*,*,#10073,.T.);
#13020=ORIENTED_EDGE('',*,*,#9983,.T.);
#13021=ORIENTED_EDGE('',*,*,#9980,.F.);
#13022=ORIENTED_EDGE('',*,*,#9977,.T.);
#13023=ORIENTED_EDGE('',*,*,#9973,.F.);
#13024=ORIENTED_EDGE('',*,*,#10049,.T.);
#13025=ORIENTED_EDGE('',*,*,#10066,.T.);
#13026=ORIENTED_EDGE('',*,*,#10072,.T.);
#13027=ORIENTED_EDGE('',*,*,#10070,.T.);
#13028=ORIENTED_EDGE('',*,*,#10074,.T.);
#13029=ORIENTED_EDGE('',*,*,#10050,.T.);
#13030=ORIENTED_EDGE('',*,*,#10035,.T.);
#13031=ORIENTED_EDGE('',*,*,#10032,.F.);
#13032=ORIENTED_EDGE('',*,*,#10029,.T.);
#13033=ORIENTED_EDGE('',*,*,#10025,.F.);
#13034=ORIENTED_EDGE('',*,*,#10075,.T.);
#13035=ORIENTED_EDGE('',*,*,#10076,.T.);
#13036=ORIENTED_EDGE('',*,*,#10076,.F.);
#13037=ORIENTED_EDGE('',*,*,#10077,.T.);
#13038=ORIENTED_EDGE('',*,*,#10078,.F.);
#13039=ORIENTED_EDGE('',*,*,#10077,.F.);
#13040=ORIENTED_EDGE('',*,*,#10079,.F.);
#13041=ORIENTED_EDGE('',*,*,#10080,.T.);
#13042=ORIENTED_EDGE('',*,*,#10075,.F.);
#13043=ORIENTED_EDGE('',*,*,#10080,.F.);
#13044=ORIENTED_EDGE('',*,*,#10079,.T.);
#13045=ORIENTED_EDGE('',*,*,#10078,.T.);
#13046=ORIENTED_EDGE('',*,*,#10081,.F.);
#13047=ORIENTED_EDGE('',*,*,#10082,.T.);
#13048=ORIENTED_EDGE('',*,*,#10083,.F.);
#13049=ORIENTED_EDGE('',*,*,#10084,.T.);
#13050=ORIENTED_EDGE('',*,*,#10085,.F.);
#13051=ORIENTED_EDGE('',*,*,#10086,.F.);
#13052=ORIENTED_EDGE('',*,*,#10087,.F.);
#13053=ORIENTED_EDGE('',*,*,#10088,.T.);
#13054=ORIENTED_EDGE('',*,*,#10089,.T.);
#13055=ORIENTED_EDGE('',*,*,#10090,.T.);
#13056=ORIENTED_EDGE('',*,*,#10091,.T.);
#13057=ORIENTED_EDGE('',*,*,#10092,.T.);
#13058=ORIENTED_EDGE('',*,*,#10093,.F.);
#13059=ORIENTED_EDGE('',*,*,#10088,.F.);
#13060=ORIENTED_EDGE('',*,*,#10094,.F.);
#13061=ORIENTED_EDGE('',*,*,#10095,.F.);
#13062=ORIENTED_EDGE('',*,*,#10087,.T.);
#13063=ORIENTED_EDGE('',*,*,#10096,.T.);
#13064=ORIENTED_EDGE('',*,*,#10097,.T.);
#13065=ORIENTED_EDGE('',*,*,#10094,.T.);
#13066=ORIENTED_EDGE('',*,*,#10098,.F.);
#13067=ORIENTED_EDGE('',*,*,#10099,.T.);
#13068=ORIENTED_EDGE('',*,*,#10096,.F.);
#13069=ORIENTED_EDGE('',*,*,#10086,.T.);
#13070=ORIENTED_EDGE('',*,*,#10100,.T.);
#13071=ORIENTED_EDGE('',*,*,#10098,.T.);
#13072=ORIENTED_EDGE('',*,*,#10085,.T.);
#13073=ORIENTED_EDGE('',*,*,#10101,.T.);
#13074=ORIENTED_EDGE('',*,*,#10102,.F.);
#13075=ORIENTED_EDGE('',*,*,#10103,.F.);
#13076=ORIENTED_EDGE('',*,*,#10101,.F.);
#13077=ORIENTED_EDGE('',*,*,#10084,.F.);
#13078=ORIENTED_EDGE('',*,*,#10083,.T.);
#13079=ORIENTED_EDGE('',*,*,#10104,.T.);
#13080=ORIENTED_EDGE('',*,*,#10105,.T.);
#13081=ORIENTED_EDGE('',*,*,#10102,.T.);
#13082=ORIENTED_EDGE('',*,*,#10106,.F.);
#13083=ORIENTED_EDGE('',*,*,#10095,.T.);
#13084=ORIENTED_EDGE('',*,*,#10097,.F.);
#13085=ORIENTED_EDGE('',*,*,#10099,.F.);
#13086=ORIENTED_EDGE('',*,*,#10100,.F.);
#13087=ORIENTED_EDGE('',*,*,#10103,.T.);
#13088=ORIENTED_EDGE('',*,*,#10105,.F.);
#13089=ORIENTED_EDGE('',*,*,#10107,.T.);
#13090=ORIENTED_EDGE('',*,*,#10108,.F.);
#13091=ORIENTED_EDGE('',*,*,#10107,.F.);
#13092=ORIENTED_EDGE('',*,*,#10104,.F.);
#13093=ORIENTED_EDGE('',*,*,#10082,.F.);
#13094=ORIENTED_EDGE('',*,*,#10106,.T.);
#13095=ORIENTED_EDGE('',*,*,#10108,.T.);
#13096=ORIENTED_EDGE('',*,*,#10081,.T.);
#13097=ORIENTED_EDGE('',*,*,#10093,.T.);
#13098=ORIENTED_EDGE('',*,*,#10091,.F.);
#13099=ORIENTED_EDGE('',*,*,#10109,.F.);
#13100=ORIENTED_EDGE('',*,*,#10110,.T.);
#13101=ORIENTED_EDGE('',*,*,#10111,.T.);
#13102=ORIENTED_EDGE('',*,*,#10090,.F.);
#13103=ORIENTED_EDGE('',*,*,#10112,.F.);
#13104=ORIENTED_EDGE('',*,*,#10113,.T.);
#13105=ORIENTED_EDGE('',*,*,#10109,.T.);
#13106=ORIENTED_EDGE('',*,*,#10092,.F.);
#13107=ORIENTED_EDGE('',*,*,#10111,.F.);
#13108=ORIENTED_EDGE('',*,*,#10114,.T.);
#13109=ORIENTED_EDGE('',*,*,#10115,.T.);
#13110=ORIENTED_EDGE('',*,*,#10089,.F.);
#13111=ORIENTED_EDGE('',*,*,#10115,.F.);
#13112=ORIENTED_EDGE('',*,*,#10116,.T.);
#13113=ORIENTED_EDGE('',*,*,#10112,.T.);
#13114=ORIENTED_EDGE('',*,*,#10117,.F.);
#13115=ORIENTED_EDGE('',*,*,#10118,.T.);
#13116=ORIENTED_EDGE('',*,*,#10119,.F.);
#13117=ORIENTED_EDGE('',*,*,#10120,.T.);
#13118=ORIENTED_EDGE('',*,*,#10121,.F.);
#13119=ORIENTED_EDGE('',*,*,#10122,.F.);
#13120=ORIENTED_EDGE('',*,*,#10123,.F.);
#13121=ORIENTED_EDGE('',*,*,#10124,.T.);
#13122=ORIENTED_EDGE('',*,*,#10125,.T.);
#13123=ORIENTED_EDGE('',*,*,#10126,.T.);
#13124=ORIENTED_EDGE('',*,*,#10127,.T.);
#13125=ORIENTED_EDGE('',*,*,#10128,.T.);
#13126=ORIENTED_EDGE('',*,*,#10129,.F.);
#13127=ORIENTED_EDGE('',*,*,#10124,.F.);
#13128=ORIENTED_EDGE('',*,*,#10130,.F.);
#13129=ORIENTED_EDGE('',*,*,#10131,.F.);
#13130=ORIENTED_EDGE('',*,*,#10123,.T.);
#13131=ORIENTED_EDGE('',*,*,#10132,.T.);
#13132=ORIENTED_EDGE('',*,*,#10133,.T.);
#13133=ORIENTED_EDGE('',*,*,#10130,.T.);
#13134=ORIENTED_EDGE('',*,*,#10134,.F.);
#13135=ORIENTED_EDGE('',*,*,#10135,.T.);
#13136=ORIENTED_EDGE('',*,*,#10132,.F.);
#13137=ORIENTED_EDGE('',*,*,#10122,.T.);
#13138=ORIENTED_EDGE('',*,*,#10136,.T.);
#13139=ORIENTED_EDGE('',*,*,#10134,.T.);
#13140=ORIENTED_EDGE('',*,*,#10121,.T.);
#13141=ORIENTED_EDGE('',*,*,#10137,.T.);
#13142=ORIENTED_EDGE('',*,*,#10138,.F.);
#13143=ORIENTED_EDGE('',*,*,#10139,.F.);
#13144=ORIENTED_EDGE('',*,*,#10137,.F.);
#13145=ORIENTED_EDGE('',*,*,#10120,.F.);
#13146=ORIENTED_EDGE('',*,*,#10119,.T.);
#13147=ORIENTED_EDGE('',*,*,#10140,.T.);
#13148=ORIENTED_EDGE('',*,*,#10141,.T.);
#13149=ORIENTED_EDGE('',*,*,#10138,.T.);
#13150=ORIENTED_EDGE('',*,*,#10142,.F.);
#13151=ORIENTED_EDGE('',*,*,#10131,.T.);
#13152=ORIENTED_EDGE('',*,*,#10133,.F.);
#13153=ORIENTED_EDGE('',*,*,#10135,.F.);
#13154=ORIENTED_EDGE('',*,*,#10136,.F.);
#13155=ORIENTED_EDGE('',*,*,#10139,.T.);
#13156=ORIENTED_EDGE('',*,*,#10141,.F.);
#13157=ORIENTED_EDGE('',*,*,#10143,.T.);
#13158=ORIENTED_EDGE('',*,*,#10144,.F.);
#13159=ORIENTED_EDGE('',*,*,#10143,.F.);
#13160=ORIENTED_EDGE('',*,*,#10140,.F.);
#13161=ORIENTED_EDGE('',*,*,#10118,.F.);
#13162=ORIENTED_EDGE('',*,*,#10142,.T.);
#13163=ORIENTED_EDGE('',*,*,#10144,.T.);
#13164=ORIENTED_EDGE('',*,*,#10117,.T.);
#13165=ORIENTED_EDGE('',*,*,#10129,.T.);
#13166=ORIENTED_EDGE('',*,*,#10127,.F.);
#13167=ORIENTED_EDGE('',*,*,#10145,.F.);
#13168=ORIENTED_EDGE('',*,*,#10146,.T.);
#13169=ORIENTED_EDGE('',*,*,#10147,.T.);
#13170=ORIENTED_EDGE('',*,*,#10126,.F.);
#13171=ORIENTED_EDGE('',*,*,#10148,.F.);
#13172=ORIENTED_EDGE('',*,*,#10149,.T.);
#13173=ORIENTED_EDGE('',*,*,#10145,.T.);
#13174=ORIENTED_EDGE('',*,*,#10128,.F.);
#13175=ORIENTED_EDGE('',*,*,#10147,.F.);
#13176=ORIENTED_EDGE('',*,*,#10150,.T.);
#13177=ORIENTED_EDGE('',*,*,#10151,.T.);
#13178=ORIENTED_EDGE('',*,*,#10125,.F.);
#13179=ORIENTED_EDGE('',*,*,#10151,.F.);
#13180=ORIENTED_EDGE('',*,*,#10152,.T.);
#13181=ORIENTED_EDGE('',*,*,#10148,.T.);
#13182=ORIENTED_EDGE('',*,*,#10153,.F.);
#13183=ORIENTED_EDGE('',*,*,#10154,.T.);
#13184=ORIENTED_EDGE('',*,*,#10155,.F.);
#13185=ORIENTED_EDGE('',*,*,#10156,.T.);
#13186=ORIENTED_EDGE('',*,*,#10157,.F.);
#13187=ORIENTED_EDGE('',*,*,#10158,.F.);
#13188=ORIENTED_EDGE('',*,*,#10159,.F.);
#13189=ORIENTED_EDGE('',*,*,#10160,.T.);
#13190=ORIENTED_EDGE('',*,*,#10161,.T.);
#13191=ORIENTED_EDGE('',*,*,#10162,.T.);
#13192=ORIENTED_EDGE('',*,*,#10163,.T.);
#13193=ORIENTED_EDGE('',*,*,#10164,.T.);
#13194=ORIENTED_EDGE('',*,*,#10165,.F.);
#13195=ORIENTED_EDGE('',*,*,#10160,.F.);
#13196=ORIENTED_EDGE('',*,*,#10166,.F.);
#13197=ORIENTED_EDGE('',*,*,#10167,.F.);
#13198=ORIENTED_EDGE('',*,*,#10159,.T.);
#13199=ORIENTED_EDGE('',*,*,#10168,.T.);
#13200=ORIENTED_EDGE('',*,*,#10169,.T.);
#13201=ORIENTED_EDGE('',*,*,#10166,.T.);
#13202=ORIENTED_EDGE('',*,*,#10170,.F.);
#13203=ORIENTED_EDGE('',*,*,#10171,.T.);
#13204=ORIENTED_EDGE('',*,*,#10168,.F.);
#13205=ORIENTED_EDGE('',*,*,#10158,.T.);
#13206=ORIENTED_EDGE('',*,*,#10172,.T.);
#13207=ORIENTED_EDGE('',*,*,#10170,.T.);
#13208=ORIENTED_EDGE('',*,*,#10157,.T.);
#13209=ORIENTED_EDGE('',*,*,#10173,.T.);
#13210=ORIENTED_EDGE('',*,*,#10174,.F.);
#13211=ORIENTED_EDGE('',*,*,#10175,.F.);
#13212=ORIENTED_EDGE('',*,*,#10173,.F.);
#13213=ORIENTED_EDGE('',*,*,#10156,.F.);
#13214=ORIENTED_EDGE('',*,*,#10155,.T.);
#13215=ORIENTED_EDGE('',*,*,#10176,.T.);
#13216=ORIENTED_EDGE('',*,*,#10177,.T.);
#13217=ORIENTED_EDGE('',*,*,#10174,.T.);
#13218=ORIENTED_EDGE('',*,*,#10178,.F.);
#13219=ORIENTED_EDGE('',*,*,#10167,.T.);
#13220=ORIENTED_EDGE('',*,*,#10169,.F.);
#13221=ORIENTED_EDGE('',*,*,#10171,.F.);
#13222=ORIENTED_EDGE('',*,*,#10172,.F.);
#13223=ORIENTED_EDGE('',*,*,#10175,.T.);
#13224=ORIENTED_EDGE('',*,*,#10177,.F.);
#13225=ORIENTED_EDGE('',*,*,#10179,.T.);
#13226=ORIENTED_EDGE('',*,*,#10180,.F.);
#13227=ORIENTED_EDGE('',*,*,#10179,.F.);
#13228=ORIENTED_EDGE('',*,*,#10176,.F.);
#13229=ORIENTED_EDGE('',*,*,#10154,.F.);
#13230=ORIENTED_EDGE('',*,*,#10178,.T.);
#13231=ORIENTED_EDGE('',*,*,#10180,.T.);
#13232=ORIENTED_EDGE('',*,*,#10153,.T.);
#13233=ORIENTED_EDGE('',*,*,#10165,.T.);
#13234=ORIENTED_EDGE('',*,*,#10163,.F.);
#13235=ORIENTED_EDGE('',*,*,#10181,.F.);
#13236=ORIENTED_EDGE('',*,*,#10182,.T.);
#13237=ORIENTED_EDGE('',*,*,#10183,.T.);
#13238=ORIENTED_EDGE('',*,*,#10162,.F.);
#13239=ORIENTED_EDGE('',*,*,#10184,.F.);
#13240=ORIENTED_EDGE('',*,*,#10185,.T.);
#13241=ORIENTED_EDGE('',*,*,#10181,.T.);
#13242=ORIENTED_EDGE('',*,*,#10164,.F.);
#13243=ORIENTED_EDGE('',*,*,#10183,.F.);
#13244=ORIENTED_EDGE('',*,*,#10186,.T.);
#13245=ORIENTED_EDGE('',*,*,#10187,.T.);
#13246=ORIENTED_EDGE('',*,*,#10161,.F.);
#13247=ORIENTED_EDGE('',*,*,#10187,.F.);
#13248=ORIENTED_EDGE('',*,*,#10188,.T.);
#13249=ORIENTED_EDGE('',*,*,#10184,.T.);
#13250=ORIENTED_EDGE('',*,*,#10189,.F.);
#13251=ORIENTED_EDGE('',*,*,#10190,.T.);
#13252=ORIENTED_EDGE('',*,*,#10191,.F.);
#13253=ORIENTED_EDGE('',*,*,#10192,.T.);
#13254=ORIENTED_EDGE('',*,*,#10193,.F.);
#13255=ORIENTED_EDGE('',*,*,#10194,.F.);
#13256=ORIENTED_EDGE('',*,*,#10195,.F.);
#13257=ORIENTED_EDGE('',*,*,#10196,.T.);
#13258=ORIENTED_EDGE('',*,*,#10197,.T.);
#13259=ORIENTED_EDGE('',*,*,#10198,.T.);
#13260=ORIENTED_EDGE('',*,*,#10199,.T.);
#13261=ORIENTED_EDGE('',*,*,#10200,.T.);
#13262=ORIENTED_EDGE('',*,*,#10201,.F.);
#13263=ORIENTED_EDGE('',*,*,#10196,.F.);
#13264=ORIENTED_EDGE('',*,*,#10202,.F.);
#13265=ORIENTED_EDGE('',*,*,#10203,.F.);
#13266=ORIENTED_EDGE('',*,*,#10195,.T.);
#13267=ORIENTED_EDGE('',*,*,#10204,.T.);
#13268=ORIENTED_EDGE('',*,*,#10205,.T.);
#13269=ORIENTED_EDGE('',*,*,#10202,.T.);
#13270=ORIENTED_EDGE('',*,*,#10206,.F.);
#13271=ORIENTED_EDGE('',*,*,#10207,.T.);
#13272=ORIENTED_EDGE('',*,*,#10204,.F.);
#13273=ORIENTED_EDGE('',*,*,#10194,.T.);
#13274=ORIENTED_EDGE('',*,*,#10208,.T.);
#13275=ORIENTED_EDGE('',*,*,#10206,.T.);
#13276=ORIENTED_EDGE('',*,*,#10193,.T.);
#13277=ORIENTED_EDGE('',*,*,#10209,.T.);
#13278=ORIENTED_EDGE('',*,*,#10210,.F.);
#13279=ORIENTED_EDGE('',*,*,#10211,.F.);
#13280=ORIENTED_EDGE('',*,*,#10209,.F.);
#13281=ORIENTED_EDGE('',*,*,#10192,.F.);
#13282=ORIENTED_EDGE('',*,*,#10191,.T.);
#13283=ORIENTED_EDGE('',*,*,#10212,.T.);
#13284=ORIENTED_EDGE('',*,*,#10213,.T.);
#13285=ORIENTED_EDGE('',*,*,#10210,.T.);
#13286=ORIENTED_EDGE('',*,*,#10214,.F.);
#13287=ORIENTED_EDGE('',*,*,#10203,.T.);
#13288=ORIENTED_EDGE('',*,*,#10205,.F.);
#13289=ORIENTED_EDGE('',*,*,#10207,.F.);
#13290=ORIENTED_EDGE('',*,*,#10208,.F.);
#13291=ORIENTED_EDGE('',*,*,#10211,.T.);
#13292=ORIENTED_EDGE('',*,*,#10213,.F.);
#13293=ORIENTED_EDGE('',*,*,#10215,.T.);
#13294=ORIENTED_EDGE('',*,*,#10216,.F.);
#13295=ORIENTED_EDGE('',*,*,#10215,.F.);
#13296=ORIENTED_EDGE('',*,*,#10212,.F.);
#13297=ORIENTED_EDGE('',*,*,#10190,.F.);
#13298=ORIENTED_EDGE('',*,*,#10214,.T.);
#13299=ORIENTED_EDGE('',*,*,#10216,.T.);
#13300=ORIENTED_EDGE('',*,*,#10189,.T.);
#13301=ORIENTED_EDGE('',*,*,#10201,.T.);
#13302=ORIENTED_EDGE('',*,*,#10199,.F.);
#13303=ORIENTED_EDGE('',*,*,#10217,.F.);
#13304=ORIENTED_EDGE('',*,*,#10218,.T.);
#13305=ORIENTED_EDGE('',*,*,#10219,.T.);
#13306=ORIENTED_EDGE('',*,*,#10198,.F.);
#13307=ORIENTED_EDGE('',*,*,#10220,.F.);
#13308=ORIENTED_EDGE('',*,*,#10221,.T.);
#13309=ORIENTED_EDGE('',*,*,#10217,.T.);
#13310=ORIENTED_EDGE('',*,*,#10200,.F.);
#13311=ORIENTED_EDGE('',*,*,#10219,.F.);
#13312=ORIENTED_EDGE('',*,*,#10222,.T.);
#13313=ORIENTED_EDGE('',*,*,#10223,.T.);
#13314=ORIENTED_EDGE('',*,*,#10197,.F.);
#13315=ORIENTED_EDGE('',*,*,#10223,.F.);
#13316=ORIENTED_EDGE('',*,*,#10224,.T.);
#13317=ORIENTED_EDGE('',*,*,#10220,.T.);
#13318=ORIENTED_EDGE('',*,*,#10225,.F.);
#13319=ORIENTED_EDGE('',*,*,#10226,.T.);
#13320=ORIENTED_EDGE('',*,*,#10227,.F.);
#13321=ORIENTED_EDGE('',*,*,#10228,.T.);
#13322=ORIENTED_EDGE('',*,*,#10229,.F.);
#13323=ORIENTED_EDGE('',*,*,#10230,.F.);
#13324=ORIENTED_EDGE('',*,*,#10231,.F.);
#13325=ORIENTED_EDGE('',*,*,#10232,.T.);
#13326=ORIENTED_EDGE('',*,*,#10233,.T.);
#13327=ORIENTED_EDGE('',*,*,#10234,.T.);
#13328=ORIENTED_EDGE('',*,*,#10235,.T.);
#13329=ORIENTED_EDGE('',*,*,#10236,.T.);
#13330=ORIENTED_EDGE('',*,*,#10237,.F.);
#13331=ORIENTED_EDGE('',*,*,#10232,.F.);
#13332=ORIENTED_EDGE('',*,*,#10238,.F.);
#13333=ORIENTED_EDGE('',*,*,#10239,.F.);
#13334=ORIENTED_EDGE('',*,*,#10231,.T.);
#13335=ORIENTED_EDGE('',*,*,#10240,.T.);
#13336=ORIENTED_EDGE('',*,*,#10241,.T.);
#13337=ORIENTED_EDGE('',*,*,#10238,.T.);
#13338=ORIENTED_EDGE('',*,*,#10242,.F.);
#13339=ORIENTED_EDGE('',*,*,#10243,.T.);
#13340=ORIENTED_EDGE('',*,*,#10240,.F.);
#13341=ORIENTED_EDGE('',*,*,#10230,.T.);
#13342=ORIENTED_EDGE('',*,*,#10244,.T.);
#13343=ORIENTED_EDGE('',*,*,#10242,.T.);
#13344=ORIENTED_EDGE('',*,*,#10229,.T.);
#13345=ORIENTED_EDGE('',*,*,#10245,.T.);
#13346=ORIENTED_EDGE('',*,*,#10246,.F.);
#13347=ORIENTED_EDGE('',*,*,#10247,.F.);
#13348=ORIENTED_EDGE('',*,*,#10245,.F.);
#13349=ORIENTED_EDGE('',*,*,#10228,.F.);
#13350=ORIENTED_EDGE('',*,*,#10227,.T.);
#13351=ORIENTED_EDGE('',*,*,#10248,.T.);
#13352=ORIENTED_EDGE('',*,*,#10249,.T.);
#13353=ORIENTED_EDGE('',*,*,#10246,.T.);
#13354=ORIENTED_EDGE('',*,*,#10250,.F.);
#13355=ORIENTED_EDGE('',*,*,#10239,.T.);
#13356=ORIENTED_EDGE('',*,*,#10241,.F.);
#13357=ORIENTED_EDGE('',*,*,#10243,.F.);
#13358=ORIENTED_EDGE('',*,*,#10244,.F.);
#13359=ORIENTED_EDGE('',*,*,#10247,.T.);
#13360=ORIENTED_EDGE('',*,*,#10249,.F.);
#13361=ORIENTED_EDGE('',*,*,#10251,.T.);
#13362=ORIENTED_EDGE('',*,*,#10252,.F.);
#13363=ORIENTED_EDGE('',*,*,#10251,.F.);
#13364=ORIENTED_EDGE('',*,*,#10248,.F.);
#13365=ORIENTED_EDGE('',*,*,#10226,.F.);
#13366=ORIENTED_EDGE('',*,*,#10250,.T.);
#13367=ORIENTED_EDGE('',*,*,#10252,.T.);
#13368=ORIENTED_EDGE('',*,*,#10225,.T.);
#13369=ORIENTED_EDGE('',*,*,#10237,.T.);
#13370=ORIENTED_EDGE('',*,*,#10235,.F.);
#13371=ORIENTED_EDGE('',*,*,#10253,.F.);
#13372=ORIENTED_EDGE('',*,*,#10254,.T.);
#13373=ORIENTED_EDGE('',*,*,#10255,.T.);
#13374=ORIENTED_EDGE('',*,*,#10234,.F.);
#13375=ORIENTED_EDGE('',*,*,#10256,.F.);
#13376=ORIENTED_EDGE('',*,*,#10257,.T.);
#13377=ORIENTED_EDGE('',*,*,#10253,.T.);
#13378=ORIENTED_EDGE('',*,*,#10236,.F.);
#13379=ORIENTED_EDGE('',*,*,#10255,.F.);
#13380=ORIENTED_EDGE('',*,*,#10258,.T.);
#13381=ORIENTED_EDGE('',*,*,#10259,.T.);
#13382=ORIENTED_EDGE('',*,*,#10233,.F.);
#13383=ORIENTED_EDGE('',*,*,#10259,.F.);
#13384=ORIENTED_EDGE('',*,*,#10260,.T.);
#13385=ORIENTED_EDGE('',*,*,#10256,.T.);
#13386=ORIENTED_EDGE('',*,*,#10261,.F.);
#13387=ORIENTED_EDGE('',*,*,#10262,.T.);
#13388=ORIENTED_EDGE('',*,*,#10263,.F.);
#13389=ORIENTED_EDGE('',*,*,#10264,.T.);
#13390=ORIENTED_EDGE('',*,*,#10265,.F.);
#13391=ORIENTED_EDGE('',*,*,#10266,.F.);
#13392=ORIENTED_EDGE('',*,*,#10267,.F.);
#13393=ORIENTED_EDGE('',*,*,#10268,.T.);
#13394=ORIENTED_EDGE('',*,*,#10269,.T.);
#13395=ORIENTED_EDGE('',*,*,#10270,.T.);
#13396=ORIENTED_EDGE('',*,*,#10271,.T.);
#13397=ORIENTED_EDGE('',*,*,#10272,.T.);
#13398=ORIENTED_EDGE('',*,*,#10273,.F.);
#13399=ORIENTED_EDGE('',*,*,#10268,.F.);
#13400=ORIENTED_EDGE('',*,*,#10274,.F.);
#13401=ORIENTED_EDGE('',*,*,#10275,.F.);
#13402=ORIENTED_EDGE('',*,*,#10267,.T.);
#13403=ORIENTED_EDGE('',*,*,#10276,.T.);
#13404=ORIENTED_EDGE('',*,*,#10277,.T.);
#13405=ORIENTED_EDGE('',*,*,#10274,.T.);
#13406=ORIENTED_EDGE('',*,*,#10278,.F.);
#13407=ORIENTED_EDGE('',*,*,#10279,.T.);
#13408=ORIENTED_EDGE('',*,*,#10276,.F.);
#13409=ORIENTED_EDGE('',*,*,#10266,.T.);
#13410=ORIENTED_EDGE('',*,*,#10280,.T.);
#13411=ORIENTED_EDGE('',*,*,#10278,.T.);
#13412=ORIENTED_EDGE('',*,*,#10265,.T.);
#13413=ORIENTED_EDGE('',*,*,#10281,.T.);
#13414=ORIENTED_EDGE('',*,*,#10282,.F.);
#13415=ORIENTED_EDGE('',*,*,#10283,.F.);
#13416=ORIENTED_EDGE('',*,*,#10281,.F.);
#13417=ORIENTED_EDGE('',*,*,#10264,.F.);
#13418=ORIENTED_EDGE('',*,*,#10263,.T.);
#13419=ORIENTED_EDGE('',*,*,#10284,.T.);
#13420=ORIENTED_EDGE('',*,*,#10285,.T.);
#13421=ORIENTED_EDGE('',*,*,#10282,.T.);
#13422=ORIENTED_EDGE('',*,*,#10286,.F.);
#13423=ORIENTED_EDGE('',*,*,#10275,.T.);
#13424=ORIENTED_EDGE('',*,*,#10277,.F.);
#13425=ORIENTED_EDGE('',*,*,#10279,.F.);
#13426=ORIENTED_EDGE('',*,*,#10280,.F.);
#13427=ORIENTED_EDGE('',*,*,#10283,.T.);
#13428=ORIENTED_EDGE('',*,*,#10285,.F.);
#13429=ORIENTED_EDGE('',*,*,#10287,.T.);
#13430=ORIENTED_EDGE('',*,*,#10288,.F.);
#13431=ORIENTED_EDGE('',*,*,#10287,.F.);
#13432=ORIENTED_EDGE('',*,*,#10284,.F.);
#13433=ORIENTED_EDGE('',*,*,#10262,.F.);
#13434=ORIENTED_EDGE('',*,*,#10286,.T.);
#13435=ORIENTED_EDGE('',*,*,#10288,.T.);
#13436=ORIENTED_EDGE('',*,*,#10261,.T.);
#13437=ORIENTED_EDGE('',*,*,#10273,.T.);
#13438=ORIENTED_EDGE('',*,*,#10271,.F.);
#13439=ORIENTED_EDGE('',*,*,#10289,.F.);
#13440=ORIENTED_EDGE('',*,*,#10290,.T.);
#13441=ORIENTED_EDGE('',*,*,#10291,.T.);
#13442=ORIENTED_EDGE('',*,*,#10270,.F.);
#13443=ORIENTED_EDGE('',*,*,#10292,.F.);
#13444=ORIENTED_EDGE('',*,*,#10293,.T.);
#13445=ORIENTED_EDGE('',*,*,#10289,.T.);
#13446=ORIENTED_EDGE('',*,*,#10272,.F.);
#13447=ORIENTED_EDGE('',*,*,#10291,.F.);
#13448=ORIENTED_EDGE('',*,*,#10294,.T.);
#13449=ORIENTED_EDGE('',*,*,#10295,.T.);
#13450=ORIENTED_EDGE('',*,*,#10269,.F.);
#13451=ORIENTED_EDGE('',*,*,#10295,.F.);
#13452=ORIENTED_EDGE('',*,*,#10296,.T.);
#13453=ORIENTED_EDGE('',*,*,#10292,.T.);
#13454=ORIENTED_EDGE('',*,*,#10297,.F.);
#13455=ORIENTED_EDGE('',*,*,#10298,.T.);
#13456=ORIENTED_EDGE('',*,*,#10299,.F.);
#13457=ORIENTED_EDGE('',*,*,#10300,.T.);
#13458=ORIENTED_EDGE('',*,*,#10301,.F.);
#13459=ORIENTED_EDGE('',*,*,#10302,.F.);
#13460=ORIENTED_EDGE('',*,*,#10303,.F.);
#13461=ORIENTED_EDGE('',*,*,#10304,.T.);
#13462=ORIENTED_EDGE('',*,*,#10305,.T.);
#13463=ORIENTED_EDGE('',*,*,#10306,.T.);
#13464=ORIENTED_EDGE('',*,*,#10307,.T.);
#13465=ORIENTED_EDGE('',*,*,#10308,.T.);
#13466=ORIENTED_EDGE('',*,*,#10309,.F.);
#13467=ORIENTED_EDGE('',*,*,#10304,.F.);
#13468=ORIENTED_EDGE('',*,*,#10310,.F.);
#13469=ORIENTED_EDGE('',*,*,#10311,.F.);
#13470=ORIENTED_EDGE('',*,*,#10303,.T.);
#13471=ORIENTED_EDGE('',*,*,#10312,.T.);
#13472=ORIENTED_EDGE('',*,*,#10313,.T.);
#13473=ORIENTED_EDGE('',*,*,#10310,.T.);
#13474=ORIENTED_EDGE('',*,*,#10314,.F.);
#13475=ORIENTED_EDGE('',*,*,#10315,.T.);
#13476=ORIENTED_EDGE('',*,*,#10312,.F.);
#13477=ORIENTED_EDGE('',*,*,#10302,.T.);
#13478=ORIENTED_EDGE('',*,*,#10316,.T.);
#13479=ORIENTED_EDGE('',*,*,#10314,.T.);
#13480=ORIENTED_EDGE('',*,*,#10301,.T.);
#13481=ORIENTED_EDGE('',*,*,#10317,.T.);
#13482=ORIENTED_EDGE('',*,*,#10318,.F.);
#13483=ORIENTED_EDGE('',*,*,#10319,.F.);
#13484=ORIENTED_EDGE('',*,*,#10317,.F.);
#13485=ORIENTED_EDGE('',*,*,#10300,.F.);
#13486=ORIENTED_EDGE('',*,*,#10299,.T.);
#13487=ORIENTED_EDGE('',*,*,#10320,.T.);
#13488=ORIENTED_EDGE('',*,*,#10321,.T.);
#13489=ORIENTED_EDGE('',*,*,#10318,.T.);
#13490=ORIENTED_EDGE('',*,*,#10322,.F.);
#13491=ORIENTED_EDGE('',*,*,#10311,.T.);
#13492=ORIENTED_EDGE('',*,*,#10313,.F.);
#13493=ORIENTED_EDGE('',*,*,#10315,.F.);
#13494=ORIENTED_EDGE('',*,*,#10316,.F.);
#13495=ORIENTED_EDGE('',*,*,#10319,.T.);
#13496=ORIENTED_EDGE('',*,*,#10321,.F.);
#13497=ORIENTED_EDGE('',*,*,#10323,.T.);
#13498=ORIENTED_EDGE('',*,*,#10324,.F.);
#13499=ORIENTED_EDGE('',*,*,#10323,.F.);
#13500=ORIENTED_EDGE('',*,*,#10320,.F.);
#13501=ORIENTED_EDGE('',*,*,#10298,.F.);
#13502=ORIENTED_EDGE('',*,*,#10322,.T.);
#13503=ORIENTED_EDGE('',*,*,#10324,.T.);
#13504=ORIENTED_EDGE('',*,*,#10297,.T.);
#13505=ORIENTED_EDGE('',*,*,#10309,.T.);
#13506=ORIENTED_EDGE('',*,*,#10307,.F.);
#13507=ORIENTED_EDGE('',*,*,#10325,.F.);
#13508=ORIENTED_EDGE('',*,*,#10326,.T.);
#13509=ORIENTED_EDGE('',*,*,#10327,.T.);
#13510=ORIENTED_EDGE('',*,*,#10306,.F.);
#13511=ORIENTED_EDGE('',*,*,#10328,.F.);
#13512=ORIENTED_EDGE('',*,*,#10329,.T.);
#13513=ORIENTED_EDGE('',*,*,#10325,.T.);
#13514=ORIENTED_EDGE('',*,*,#10308,.F.);
#13515=ORIENTED_EDGE('',*,*,#10327,.F.);
#13516=ORIENTED_EDGE('',*,*,#10330,.T.);
#13517=ORIENTED_EDGE('',*,*,#10331,.T.);
#13518=ORIENTED_EDGE('',*,*,#10305,.F.);
#13519=ORIENTED_EDGE('',*,*,#10331,.F.);
#13520=ORIENTED_EDGE('',*,*,#10332,.T.);
#13521=ORIENTED_EDGE('',*,*,#10328,.T.);
#13522=ORIENTED_EDGE('',*,*,#10333,.F.);
#13523=ORIENTED_EDGE('',*,*,#10334,.T.);
#13524=ORIENTED_EDGE('',*,*,#10335,.F.);
#13525=ORIENTED_EDGE('',*,*,#10336,.T.);
#13526=ORIENTED_EDGE('',*,*,#10337,.F.);
#13527=ORIENTED_EDGE('',*,*,#10338,.F.);
#13528=ORIENTED_EDGE('',*,*,#10339,.F.);
#13529=ORIENTED_EDGE('',*,*,#10340,.T.);
#13530=ORIENTED_EDGE('',*,*,#10341,.T.);
#13531=ORIENTED_EDGE('',*,*,#10342,.T.);
#13532=ORIENTED_EDGE('',*,*,#10343,.T.);
#13533=ORIENTED_EDGE('',*,*,#10344,.T.);
#13534=ORIENTED_EDGE('',*,*,#10345,.F.);
#13535=ORIENTED_EDGE('',*,*,#10340,.F.);
#13536=ORIENTED_EDGE('',*,*,#10346,.F.);
#13537=ORIENTED_EDGE('',*,*,#10347,.F.);
#13538=ORIENTED_EDGE('',*,*,#10339,.T.);
#13539=ORIENTED_EDGE('',*,*,#10348,.T.);
#13540=ORIENTED_EDGE('',*,*,#10349,.T.);
#13541=ORIENTED_EDGE('',*,*,#10346,.T.);
#13542=ORIENTED_EDGE('',*,*,#10350,.F.);
#13543=ORIENTED_EDGE('',*,*,#10351,.T.);
#13544=ORIENTED_EDGE('',*,*,#10348,.F.);
#13545=ORIENTED_EDGE('',*,*,#10338,.T.);
#13546=ORIENTED_EDGE('',*,*,#10352,.T.);
#13547=ORIENTED_EDGE('',*,*,#10350,.T.);
#13548=ORIENTED_EDGE('',*,*,#10337,.T.);
#13549=ORIENTED_EDGE('',*,*,#10353,.T.);
#13550=ORIENTED_EDGE('',*,*,#10354,.F.);
#13551=ORIENTED_EDGE('',*,*,#10355,.F.);
#13552=ORIENTED_EDGE('',*,*,#10353,.F.);
#13553=ORIENTED_EDGE('',*,*,#10336,.F.);
#13554=ORIENTED_EDGE('',*,*,#10335,.T.);
#13555=ORIENTED_EDGE('',*,*,#10356,.T.);
#13556=ORIENTED_EDGE('',*,*,#10357,.T.);
#13557=ORIENTED_EDGE('',*,*,#10354,.T.);
#13558=ORIENTED_EDGE('',*,*,#10358,.F.);
#13559=ORIENTED_EDGE('',*,*,#10347,.T.);
#13560=ORIENTED_EDGE('',*,*,#10349,.F.);
#13561=ORIENTED_EDGE('',*,*,#10351,.F.);
#13562=ORIENTED_EDGE('',*,*,#10352,.F.);
#13563=ORIENTED_EDGE('',*,*,#10355,.T.);
#13564=ORIENTED_EDGE('',*,*,#10357,.F.);
#13565=ORIENTED_EDGE('',*,*,#10359,.T.);
#13566=ORIENTED_EDGE('',*,*,#10360,.F.);
#13567=ORIENTED_EDGE('',*,*,#10359,.F.);
#13568=ORIENTED_EDGE('',*,*,#10356,.F.);
#13569=ORIENTED_EDGE('',*,*,#10334,.F.);
#13570=ORIENTED_EDGE('',*,*,#10358,.T.);
#13571=ORIENTED_EDGE('',*,*,#10360,.T.);
#13572=ORIENTED_EDGE('',*,*,#10333,.T.);
#13573=ORIENTED_EDGE('',*,*,#10345,.T.);
#13574=ORIENTED_EDGE('',*,*,#10343,.F.);
#13575=ORIENTED_EDGE('',*,*,#10361,.F.);
#13576=ORIENTED_EDGE('',*,*,#10362,.T.);
#13577=ORIENTED_EDGE('',*,*,#10363,.T.);
#13578=ORIENTED_EDGE('',*,*,#10342,.F.);
#13579=ORIENTED_EDGE('',*,*,#10364,.F.);
#13580=ORIENTED_EDGE('',*,*,#10365,.T.);
#13581=ORIENTED_EDGE('',*,*,#10361,.T.);
#13582=ORIENTED_EDGE('',*,*,#10344,.F.);
#13583=ORIENTED_EDGE('',*,*,#10363,.F.);
#13584=ORIENTED_EDGE('',*,*,#10366,.T.);
#13585=ORIENTED_EDGE('',*,*,#10367,.T.);
#13586=ORIENTED_EDGE('',*,*,#10368,.T.);
#13587=ORIENTED_EDGE('',*,*,#10369,.T.);
#13588=ORIENTED_EDGE('',*,*,#10341,.F.);
#13589=ORIENTED_EDGE('',*,*,#10369,.F.);
#13590=ORIENTED_EDGE('',*,*,#10370,.T.);
#13591=ORIENTED_EDGE('',*,*,#10364,.T.);
#13592=ORIENTED_EDGE('',*,*,#10371,.T.);
#13593=ORIENTED_EDGE('',*,*,#10372,.T.);
#13594=ORIENTED_EDGE('',*,*,#10373,.T.);
#13595=ORIENTED_EDGE('',*,*,#10374,.T.);
#13596=ORIENTED_EDGE('',*,*,#10375,.T.);
#13597=ORIENTED_EDGE('',*,*,#10376,.T.);
#13598=ORIENTED_EDGE('',*,*,#10377,.T.);
#13599=ORIENTED_EDGE('',*,*,#10378,.T.);
#13600=ORIENTED_EDGE('',*,*,#10379,.T.);
#13601=ORIENTED_EDGE('',*,*,#10380,.T.);
#13602=ORIENTED_EDGE('',*,*,#10381,.T.);
#13603=ORIENTED_EDGE('',*,*,#10382,.T.);
#13604=ORIENTED_EDGE('',*,*,#10383,.T.);
#13605=ORIENTED_EDGE('',*,*,#10384,.T.);
#13606=ORIENTED_EDGE('',*,*,#10385,.T.);
#13607=ORIENTED_EDGE('',*,*,#10386,.T.);
#13608=ORIENTED_EDGE('',*,*,#10387,.T.);
#13609=ORIENTED_EDGE('',*,*,#10376,.F.);
#13610=ORIENTED_EDGE('',*,*,#10388,.T.);
#13611=ORIENTED_EDGE('',*,*,#10389,.F.);
#13612=ORIENTED_EDGE('',*,*,#10390,.T.);
#13613=ORIENTED_EDGE('',*,*,#10377,.F.);
#13614=ORIENTED_EDGE('',*,*,#10387,.F.);
#13615=ORIENTED_EDGE('',*,*,#10391,.F.);
#13616=ORIENTED_EDGE('',*,*,#10392,.T.);
#13617=ORIENTED_EDGE('',*,*,#10393,.T.);
#13618=ORIENTED_EDGE('',*,*,#10378,.F.);
#13619=ORIENTED_EDGE('',*,*,#10390,.F.);
#13620=ORIENTED_EDGE('',*,*,#10394,.F.);
#13621=ORIENTED_EDGE('',*,*,#10395,.T.);
#13622=ORIENTED_EDGE('',*,*,#10372,.F.);
#13623=ORIENTED_EDGE('',*,*,#10396,.F.);
#13624=ORIENTED_EDGE('',*,*,#10397,.F.);
#13625=ORIENTED_EDGE('',*,*,#10398,.F.);
#13626=ORIENTED_EDGE('',*,*,#10399,.T.);
#13627=ORIENTED_EDGE('',*,*,#10373,.F.);
#13628=ORIENTED_EDGE('',*,*,#10395,.F.);
#13629=ORIENTED_EDGE('',*,*,#10400,.F.);
#13630=ORIENTED_EDGE('',*,*,#10401,.T.);
#13631=ORIENTED_EDGE('',*,*,#10374,.F.);
#13632=ORIENTED_EDGE('',*,*,#10399,.F.);
#13633=ORIENTED_EDGE('',*,*,#10402,.F.);
#13634=ORIENTED_EDGE('',*,*,#10388,.F.);
#13635=ORIENTED_EDGE('',*,*,#10375,.F.);
#13636=ORIENTED_EDGE('',*,*,#10401,.F.);
#13637=ORIENTED_EDGE('',*,*,#10403,.F.);
#13638=ORIENTED_EDGE('',*,*,#10389,.T.);
#13639=ORIENTED_EDGE('',*,*,#10403,.T.);
#13640=ORIENTED_EDGE('',*,*,#10402,.T.);
#13641=ORIENTED_EDGE('',*,*,#10400,.T.);
#13642=ORIENTED_EDGE('',*,*,#10398,.T.);
#13643=ORIENTED_EDGE('',*,*,#10404,.T.);
#13644=ORIENTED_EDGE('',*,*,#10405,.F.);
#13645=ORIENTED_EDGE('',*,*,#10406,.F.);
#13646=ORIENTED_EDGE('',*,*,#10394,.T.);
#13647=ORIENTED_EDGE('',*,*,#10391,.T.);
#13648=ORIENTED_EDGE('',*,*,#10407,.T.);
#13649=ORIENTED_EDGE('',*,*,#10408,.T.);
#13650=ORIENTED_EDGE('',*,*,#10409,.T.);
#13651=ORIENTED_EDGE('',*,*,#10410,.T.);
#13652=ORIENTED_EDGE('',*,*,#10411,.T.);
#13653=ORIENTED_EDGE('',*,*,#10412,.T.);
#13654=ORIENTED_EDGE('',*,*,#10413,.T.);
#13655=ORIENTED_EDGE('',*,*,#10414,.T.);
#13656=ORIENTED_EDGE('',*,*,#10415,.T.);
#13657=ORIENTED_EDGE('',*,*,#10416,.T.);
#13658=ORIENTED_EDGE('',*,*,#10417,.T.);
#13659=ORIENTED_EDGE('',*,*,#10418,.T.);
#13660=ORIENTED_EDGE('',*,*,#10419,.F.);
#13661=ORIENTED_EDGE('',*,*,#10415,.F.);
#13662=ORIENTED_EDGE('',*,*,#10420,.T.);
#13663=ORIENTED_EDGE('',*,*,#10380,.F.);
#13664=ORIENTED_EDGE('',*,*,#10332,.F.);
#13665=ORIENTED_EDGE('',*,*,#10330,.F.);
#13666=ORIENTED_EDGE('',*,*,#10326,.F.);
#13667=ORIENTED_EDGE('',*,*,#10329,.F.);
#13668=ORIENTED_EDGE('',*,*,#10420,.F.);
#13669=ORIENTED_EDGE('',*,*,#10414,.F.);
#13670=ORIENTED_EDGE('',*,*,#10421,.F.);
#13671=ORIENTED_EDGE('',*,*,#10381,.F.);
#13672=ORIENTED_EDGE('',*,*,#10296,.F.);
#13673=ORIENTED_EDGE('',*,*,#10294,.F.);
#13674=ORIENTED_EDGE('',*,*,#10290,.F.);
#13675=ORIENTED_EDGE('',*,*,#10293,.F.);
#13676=ORIENTED_EDGE('',*,*,#10422,.T.);
#13677=ORIENTED_EDGE('',*,*,#10382,.F.);
#13678=ORIENTED_EDGE('',*,*,#10421,.T.);
#13679=ORIENTED_EDGE('',*,*,#10413,.F.);
#13680=ORIENTED_EDGE('',*,*,#10260,.F.);
#13681=ORIENTED_EDGE('',*,*,#10258,.F.);
#13682=ORIENTED_EDGE('',*,*,#10254,.F.);
#13683=ORIENTED_EDGE('',*,*,#10257,.F.);
#13684=ORIENTED_EDGE('',*,*,#10423,.T.);
#13685=ORIENTED_EDGE('',*,*,#10383,.F.);
#13686=ORIENTED_EDGE('',*,*,#10422,.F.);
#13687=ORIENTED_EDGE('',*,*,#10412,.F.);
#13688=ORIENTED_EDGE('',*,*,#10224,.F.);
#13689=ORIENTED_EDGE('',*,*,#10222,.F.);
#13690=ORIENTED_EDGE('',*,*,#10218,.F.);
#13691=ORIENTED_EDGE('',*,*,#10221,.F.);
#13692=ORIENTED_EDGE('',*,*,#10424,.T.);
#13693=ORIENTED_EDGE('',*,*,#10384,.F.);
#13694=ORIENTED_EDGE('',*,*,#10423,.F.);
#13695=ORIENTED_EDGE('',*,*,#10411,.F.);
#13696=ORIENTED_EDGE('',*,*,#10188,.F.);
#13697=ORIENTED_EDGE('',*,*,#10186,.F.);
#13698=ORIENTED_EDGE('',*,*,#10182,.F.);
#13699=ORIENTED_EDGE('',*,*,#10185,.F.);
#13700=ORIENTED_EDGE('',*,*,#10424,.F.);
#13701=ORIENTED_EDGE('',*,*,#10410,.F.);
#13702=ORIENTED_EDGE('',*,*,#10425,.T.);
#13703=ORIENTED_EDGE('',*,*,#10385,.F.);
#13704=ORIENTED_EDGE('',*,*,#10152,.F.);
#13705=ORIENTED_EDGE('',*,*,#10150,.F.);
#13706=ORIENTED_EDGE('',*,*,#10146,.F.);
#13707=ORIENTED_EDGE('',*,*,#10149,.F.);
#13708=ORIENTED_EDGE('',*,*,#10425,.F.);
#13709=ORIENTED_EDGE('',*,*,#10409,.F.);
#13710=ORIENTED_EDGE('',*,*,#10426,.T.);
#13711=ORIENTED_EDGE('',*,*,#10386,.F.);
#13712=ORIENTED_EDGE('',*,*,#10116,.F.);
#13713=ORIENTED_EDGE('',*,*,#10114,.F.);
#13714=ORIENTED_EDGE('',*,*,#10110,.F.);
#13715=ORIENTED_EDGE('',*,*,#10113,.F.);
#13716=ORIENTED_EDGE('',*,*,#10427,.F.);
#13717=ORIENTED_EDGE('',*,*,#10428,.F.);
#13718=ORIENTED_EDGE('',*,*,#10429,.F.);
#13719=ORIENTED_EDGE('',*,*,#10430,.T.);
#13720=ORIENTED_EDGE('',*,*,#10431,.F.);
#13721=ORIENTED_EDGE('',*,*,#10432,.F.);
#13722=ORIENTED_EDGE('',*,*,#10433,.F.);
#13723=ORIENTED_EDGE('',*,*,#10434,.F.);
#13724=ORIENTED_EDGE('',*,*,#10435,.F.);
#13725=ORIENTED_EDGE('',*,*,#10428,.T.);
#13726=ORIENTED_EDGE('',*,*,#10436,.F.);
#13727=ORIENTED_EDGE('',*,*,#10407,.F.);
#13728=ORIENTED_EDGE('',*,*,#10437,.T.);
#13729=ORIENTED_EDGE('',*,*,#10438,.T.);
#13730=ORIENTED_EDGE('',*,*,#10439,.F.);
#13731=ORIENTED_EDGE('',*,*,#10440,.T.);
#13732=ORIENTED_EDGE('',*,*,#10441,.F.);
#13733=ORIENTED_EDGE('',*,*,#10417,.F.);
#13734=ORIENTED_EDGE('',*,*,#10442,.F.);
#13735=ORIENTED_EDGE('',*,*,#10430,.F.);
#13736=ORIENTED_EDGE('',*,*,#10367,.F.);
#13737=ORIENTED_EDGE('',*,*,#10432,.T.);
#13738=ORIENTED_EDGE('',*,*,#10443,.T.);
#13739=ORIENTED_EDGE('',*,*,#10434,.T.);
#13740=ORIENTED_EDGE('',*,*,#10444,.T.);
#13741=ORIENTED_EDGE('',*,*,#10439,.T.);
#13742=ORIENTED_EDGE('',*,*,#10445,.T.);
#13743=ORIENTED_EDGE('',*,*,#10446,.T.);
#13744=ORIENTED_EDGE('',*,*,#10405,.T.);
#13745=ORIENTED_EDGE('',*,*,#10447,.T.);
#13746=ORIENTED_EDGE('',*,*,#10448,.F.);
#13747=ORIENTED_EDGE('',*,*,#10435,.T.);
#13748=ORIENTED_EDGE('',*,*,#10443,.F.);
#13749=ORIENTED_EDGE('',*,*,#10449,.F.);
#13750=ORIENTED_EDGE('',*,*,#10450,.F.);
#13751=ORIENTED_EDGE('',*,*,#10451,.T.);
#13752=ORIENTED_EDGE('',*,*,#10445,.F.);
#13753=ORIENTED_EDGE('',*,*,#10438,.F.);
#13754=ORIENTED_EDGE('',*,*,#10392,.F.);
#13755=ORIENTED_EDGE('',*,*,#10406,.T.);
#13756=ORIENTED_EDGE('',*,*,#10446,.F.);
#13757=ORIENTED_EDGE('',*,*,#10451,.F.);
#13758=ORIENTED_EDGE('',*,*,#10397,.T.);
#13759=ORIENTED_EDGE('',*,*,#10449,.T.);
#13760=ORIENTED_EDGE('',*,*,#10447,.F.);
#13761=ORIENTED_EDGE('',*,*,#10404,.F.);
#13762=ORIENTED_EDGE('',*,*,#10426,.F.);
#13763=ORIENTED_EDGE('',*,*,#10408,.F.);
#13764=ORIENTED_EDGE('',*,*,#10436,.T.);
#13765=ORIENTED_EDGE('',*,*,#10427,.T.);
#13766=ORIENTED_EDGE('',*,*,#10366,.F.);
#13767=ORIENTED_EDGE('',*,*,#10362,.F.);
#13768=ORIENTED_EDGE('',*,*,#10365,.F.);
#13769=ORIENTED_EDGE('',*,*,#10370,.F.);
#13770=ORIENTED_EDGE('',*,*,#10368,.F.);
#13771=ORIENTED_EDGE('',*,*,#10431,.T.);
#13772=ORIENTED_EDGE('',*,*,#10442,.T.);
#13773=ORIENTED_EDGE('',*,*,#10416,.F.);
#13774=ORIENTED_EDGE('',*,*,#10419,.T.);
#13775=ORIENTED_EDGE('',*,*,#10379,.F.);
#13776=ORIENTED_EDGE('',*,*,#10448,.T.);
#13777=ORIENTED_EDGE('',*,*,#10396,.T.);
#13778=ORIENTED_EDGE('',*,*,#10371,.F.);
#13779=ORIENTED_EDGE('',*,*,#10393,.F.);
#13780=ORIENTED_EDGE('',*,*,#10450,.T.);
#13781=ORIENTED_EDGE('',*,*,#10429,.T.);
#13782=ORIENTED_EDGE('',*,*,#10452,.T.);
#13783=ORIENTED_EDGE('',*,*,#10440,.F.);
#13784=ORIENTED_EDGE('',*,*,#10444,.F.);
#13785=ORIENTED_EDGE('',*,*,#10433,.T.);
#13786=ORIENTED_EDGE('',*,*,#10452,.F.);
#13787=ORIENTED_EDGE('',*,*,#10437,.F.);
#13788=ORIENTED_EDGE('',*,*,#10418,.F.);
#13789=ORIENTED_EDGE('',*,*,#10441,.T.);
#13790=ORIENTED_EDGE('',*,*,#10453,.F.);
#13791=ORIENTED_EDGE('',*,*,#10454,.F.);
#13792=ORIENTED_EDGE('',*,*,#10455,.F.);
#13793=ORIENTED_EDGE('',*,*,#10456,.F.);
#13794=ORIENTED_EDGE('',*,*,#10457,.F.);
#13795=ORIENTED_EDGE('',*,*,#10458,.F.);
#13796=ORIENTED_EDGE('',*,*,#10459,.F.);
#13797=ORIENTED_EDGE('',*,*,#10460,.F.);
#13798=ORIENTED_EDGE('',*,*,#10461,.F.);
#13799=ORIENTED_EDGE('',*,*,#10462,.F.);
#13800=ORIENTED_EDGE('',*,*,#10463,.F.);
#13801=ORIENTED_EDGE('',*,*,#10464,.F.);
#13802=ORIENTED_EDGE('',*,*,#10465,.F.);
#13803=ORIENTED_EDGE('',*,*,#10466,.F.);
#13804=ORIENTED_EDGE('',*,*,#10467,.F.);
#13805=ORIENTED_EDGE('',*,*,#10468,.F.);
#13806=ORIENTED_EDGE('',*,*,#10469,.F.);
#13807=ORIENTED_EDGE('',*,*,#10470,.F.);
#13808=ORIENTED_EDGE('',*,*,#10471,.F.);
#13809=ORIENTED_EDGE('',*,*,#10472,.F.);
#13810=ORIENTED_EDGE('',*,*,#10473,.F.);
#13811=ORIENTED_EDGE('',*,*,#10474,.F.);
#13812=ORIENTED_EDGE('',*,*,#10475,.F.);
#13813=ORIENTED_EDGE('',*,*,#10476,.F.);
#13814=ORIENTED_EDGE('',*,*,#10477,.F.);
#13815=ORIENTED_EDGE('',*,*,#10478,.F.);
#13816=ORIENTED_EDGE('',*,*,#10479,.F.);
#13817=ORIENTED_EDGE('',*,*,#10480,.F.);
#13818=ORIENTED_EDGE('',*,*,#10481,.F.);
#13819=ORIENTED_EDGE('',*,*,#10482,.F.);
#13820=ORIENTED_EDGE('',*,*,#10483,.F.);
#13821=ORIENTED_EDGE('',*,*,#10484,.F.);
#13822=ORIENTED_EDGE('',*,*,#10485,.F.);
#13823=ORIENTED_EDGE('',*,*,#10486,.F.);
#13824=ORIENTED_EDGE('',*,*,#10487,.F.);
#13825=ORIENTED_EDGE('',*,*,#10488,.F.);
#13826=ORIENTED_EDGE('',*,*,#10489,.F.);
#13827=ORIENTED_EDGE('',*,*,#10490,.F.);
#13828=ORIENTED_EDGE('',*,*,#10491,.F.);
#13829=ORIENTED_EDGE('',*,*,#10492,.F.);
#13830=ORIENTED_EDGE('',*,*,#10493,.F.);
#13831=ORIENTED_EDGE('',*,*,#10494,.F.);
#13832=ORIENTED_EDGE('',*,*,#10495,.F.);
#13833=ORIENTED_EDGE('',*,*,#10496,.F.);
#13834=ORIENTED_EDGE('',*,*,#10497,.F.);
#13835=ORIENTED_EDGE('',*,*,#10498,.F.);
#13836=ORIENTED_EDGE('',*,*,#10499,.F.);
#13837=ORIENTED_EDGE('',*,*,#10500,.F.);
#13838=ORIENTED_EDGE('',*,*,#10501,.F.);
#13839=ORIENTED_EDGE('',*,*,#10502,.F.);
#13840=ORIENTED_EDGE('',*,*,#10503,.F.);
#13841=ORIENTED_EDGE('',*,*,#10504,.F.);
#13842=ORIENTED_EDGE('',*,*,#10505,.F.);
#13843=ORIENTED_EDGE('',*,*,#10506,.F.);
#13844=ORIENTED_EDGE('',*,*,#10507,.F.);
#13845=ORIENTED_EDGE('',*,*,#10508,.F.);
#13846=ORIENTED_EDGE('',*,*,#10509,.F.);
#13847=ORIENTED_EDGE('',*,*,#10510,.F.);
#13848=ORIENTED_EDGE('',*,*,#10511,.F.);
#13849=ORIENTED_EDGE('',*,*,#10512,.F.);
#13850=ORIENTED_EDGE('',*,*,#10513,.F.);
#13851=ORIENTED_EDGE('',*,*,#10514,.F.);
#13852=ORIENTED_EDGE('',*,*,#10515,.F.);
#13853=ORIENTED_EDGE('',*,*,#10516,.F.);
#13854=ORIENTED_EDGE('',*,*,#10517,.F.);
#13855=ORIENTED_EDGE('',*,*,#10518,.F.);
#13856=ORIENTED_EDGE('',*,*,#10519,.F.);
#13857=ORIENTED_EDGE('',*,*,#10520,.F.);
#13858=ORIENTED_EDGE('',*,*,#10521,.F.);
#13859=ORIENTED_EDGE('',*,*,#10522,.F.);
#13860=ORIENTED_EDGE('',*,*,#10523,.F.);
#13861=ORIENTED_EDGE('',*,*,#10524,.F.);
#13862=ORIENTED_EDGE('',*,*,#10525,.F.);
#13863=ORIENTED_EDGE('',*,*,#10526,.F.);
#13864=ORIENTED_EDGE('',*,*,#10527,.F.);
#13865=ORIENTED_EDGE('',*,*,#10528,.F.);
#13866=ORIENTED_EDGE('',*,*,#10529,.F.);
#13867=ORIENTED_EDGE('',*,*,#10530,.F.);
#13868=ORIENTED_EDGE('',*,*,#10531,.F.);
#13869=ORIENTED_EDGE('',*,*,#10532,.F.);
#13870=ORIENTED_EDGE('',*,*,#10533,.F.);
#13871=ORIENTED_EDGE('',*,*,#10534,.F.);
#13872=ORIENTED_EDGE('',*,*,#10535,.F.);
#13873=ORIENTED_EDGE('',*,*,#10536,.F.);
#13874=ORIENTED_EDGE('',*,*,#10537,.F.);
#13875=ORIENTED_EDGE('',*,*,#10538,.F.);
#13876=ORIENTED_EDGE('',*,*,#10539,.F.);
#13877=ORIENTED_EDGE('',*,*,#10540,.F.);
#13878=ORIENTED_EDGE('',*,*,#10541,.F.);
#13879=ORIENTED_EDGE('',*,*,#10542,.F.);
#13880=ORIENTED_EDGE('',*,*,#10543,.F.);
#13881=ORIENTED_EDGE('',*,*,#10544,.F.);
#13882=ORIENTED_EDGE('',*,*,#10545,.F.);
#13883=ORIENTED_EDGE('',*,*,#10546,.F.);
#13884=ORIENTED_EDGE('',*,*,#10547,.F.);
#13885=ORIENTED_EDGE('',*,*,#10548,.F.);
#13886=ORIENTED_EDGE('',*,*,#10549,.F.);
#13887=ORIENTED_EDGE('',*,*,#10550,.F.);
#13888=ORIENTED_EDGE('',*,*,#10551,.F.);
#13889=ORIENTED_EDGE('',*,*,#10552,.F.);
#13890=ORIENTED_EDGE('',*,*,#10553,.F.);
#13891=ORIENTED_EDGE('',*,*,#10554,.F.);
#13892=ORIENTED_EDGE('',*,*,#10555,.F.);
#13893=ORIENTED_EDGE('',*,*,#10556,.F.);
#13894=ORIENTED_EDGE('',*,*,#10557,.F.);
#13895=ORIENTED_EDGE('',*,*,#10558,.F.);
#13896=ORIENTED_EDGE('',*,*,#10559,.F.);
#13897=ORIENTED_EDGE('',*,*,#10560,.F.);
#13898=ORIENTED_EDGE('',*,*,#10561,.F.);
#13899=ORIENTED_EDGE('',*,*,#10562,.F.);
#13900=ORIENTED_EDGE('',*,*,#10563,.F.);
#13901=ORIENTED_EDGE('',*,*,#10564,.F.);
#13902=ORIENTED_EDGE('',*,*,#10565,.F.);
#13903=ORIENTED_EDGE('',*,*,#10566,.F.);
#13904=ORIENTED_EDGE('',*,*,#10567,.F.);
#13905=ORIENTED_EDGE('',*,*,#10568,.F.);
#13906=ORIENTED_EDGE('',*,*,#10569,.F.);
#13907=ORIENTED_EDGE('',*,*,#10570,.F.);
#13908=ORIENTED_EDGE('',*,*,#10571,.F.);
#13909=ORIENTED_EDGE('',*,*,#10572,.F.);
#13910=ORIENTED_EDGE('',*,*,#10573,.F.);
#13911=ORIENTED_EDGE('',*,*,#10574,.F.);
#13912=ORIENTED_EDGE('',*,*,#10575,.F.);
#13913=ORIENTED_EDGE('',*,*,#10576,.F.);
#13914=ORIENTED_EDGE('',*,*,#10577,.F.);
#13915=ORIENTED_EDGE('',*,*,#10578,.F.);
#13916=ORIENTED_EDGE('',*,*,#10579,.F.);
#13917=ORIENTED_EDGE('',*,*,#10580,.F.);
#13918=ORIENTED_EDGE('',*,*,#10581,.F.);
#13919=ORIENTED_EDGE('',*,*,#10582,.F.);
#13920=ORIENTED_EDGE('',*,*,#10583,.F.);
#13921=ORIENTED_EDGE('',*,*,#10584,.F.);
#13922=ORIENTED_EDGE('',*,*,#10585,.F.);
#13923=ORIENTED_EDGE('',*,*,#10586,.F.);
#13924=ORIENTED_EDGE('',*,*,#10587,.F.);
#13925=ORIENTED_EDGE('',*,*,#10588,.F.);
#13926=ORIENTED_EDGE('',*,*,#10589,.F.);
#13927=ORIENTED_EDGE('',*,*,#10590,.F.);
#13928=ORIENTED_EDGE('',*,*,#10591,.F.);
#13929=ORIENTED_EDGE('',*,*,#10592,.F.);
#13930=ORIENTED_EDGE('',*,*,#10593,.F.);
#13931=ORIENTED_EDGE('',*,*,#10594,.F.);
#13932=ORIENTED_EDGE('',*,*,#10595,.F.);
#13933=ORIENTED_EDGE('',*,*,#10596,.F.);
#13934=ORIENTED_EDGE('',*,*,#10597,.F.);
#13935=ORIENTED_EDGE('',*,*,#10598,.F.);
#13936=ORIENTED_EDGE('',*,*,#10599,.F.);
#13937=ORIENTED_EDGE('',*,*,#10600,.F.);
#13938=ORIENTED_EDGE('',*,*,#10601,.F.);
#13939=ORIENTED_EDGE('',*,*,#10602,.F.);
#13940=ORIENTED_EDGE('',*,*,#10603,.F.);
#13941=ORIENTED_EDGE('',*,*,#10604,.F.);
#13942=ORIENTED_EDGE('',*,*,#10605,.F.);
#13943=ORIENTED_EDGE('',*,*,#10606,.F.);
#13944=ORIENTED_EDGE('',*,*,#10607,.F.);
#13945=ORIENTED_EDGE('',*,*,#10608,.F.);
#13946=ORIENTED_EDGE('',*,*,#10609,.F.);
#13947=ORIENTED_EDGE('',*,*,#10610,.F.);
#13948=ORIENTED_EDGE('',*,*,#10611,.F.);
#13949=ORIENTED_EDGE('',*,*,#10612,.F.);
#13950=ORIENTED_EDGE('',*,*,#10613,.F.);
#13951=ORIENTED_EDGE('',*,*,#10614,.F.);
#13952=ORIENTED_EDGE('',*,*,#10615,.F.);
#13953=ORIENTED_EDGE('',*,*,#10616,.F.);
#13954=ORIENTED_EDGE('',*,*,#10617,.F.);
#13955=ORIENTED_EDGE('',*,*,#10618,.F.);
#13956=ORIENTED_EDGE('',*,*,#10619,.F.);
#13957=ORIENTED_EDGE('',*,*,#10620,.F.);
#13958=ORIENTED_EDGE('',*,*,#10621,.F.);
#13959=ORIENTED_EDGE('',*,*,#10622,.F.);
#13960=ORIENTED_EDGE('',*,*,#10623,.F.);
#13961=ORIENTED_EDGE('',*,*,#10624,.F.);
#13962=ORIENTED_EDGE('',*,*,#10625,.F.);
#13963=ORIENTED_EDGE('',*,*,#10626,.F.);
#13964=ORIENTED_EDGE('',*,*,#10627,.F.);
#13965=ORIENTED_EDGE('',*,*,#10628,.F.);
#13966=ORIENTED_EDGE('',*,*,#10456,.T.);
#13967=ORIENTED_EDGE('',*,*,#10629,.T.);
#13968=ORIENTED_EDGE('',*,*,#10630,.T.);
#13969=ORIENTED_EDGE('',*,*,#10631,.T.);
#13970=ORIENTED_EDGE('',*,*,#10628,.T.);
#13971=ORIENTED_EDGE('',*,*,#10632,.T.);
#13972=ORIENTED_EDGE('',*,*,#10624,.T.);
#13973=ORIENTED_EDGE('',*,*,#10633,.T.);
#13974=ORIENTED_EDGE('',*,*,#10620,.T.);
#13975=ORIENTED_EDGE('',*,*,#10634,.T.);
#13976=ORIENTED_EDGE('',*,*,#10616,.T.);
#13977=ORIENTED_EDGE('',*,*,#10635,.T.);
#13978=ORIENTED_EDGE('',*,*,#10612,.T.);
#13979=ORIENTED_EDGE('',*,*,#10636,.T.);
#13980=ORIENTED_EDGE('',*,*,#10608,.T.);
#13981=ORIENTED_EDGE('',*,*,#10637,.T.);
#13982=ORIENTED_EDGE('',*,*,#10604,.T.);
#13983=ORIENTED_EDGE('',*,*,#10638,.T.);
#13984=ORIENTED_EDGE('',*,*,#10600,.T.);
#13985=ORIENTED_EDGE('',*,*,#10639,.T.);
#13986=ORIENTED_EDGE('',*,*,#10596,.T.);
#13987=ORIENTED_EDGE('',*,*,#10640,.T.);
#13988=ORIENTED_EDGE('',*,*,#10592,.T.);
#13989=ORIENTED_EDGE('',*,*,#10641,.T.);
#13990=ORIENTED_EDGE('',*,*,#10588,.T.);
#13991=ORIENTED_EDGE('',*,*,#10642,.T.);
#13992=ORIENTED_EDGE('',*,*,#10584,.T.);
#13993=ORIENTED_EDGE('',*,*,#10643,.T.);
#13994=ORIENTED_EDGE('',*,*,#10580,.T.);
#13995=ORIENTED_EDGE('',*,*,#10644,.T.);
#13996=ORIENTED_EDGE('',*,*,#10576,.T.);
#13997=ORIENTED_EDGE('',*,*,#10645,.T.);
#13998=ORIENTED_EDGE('',*,*,#10572,.T.);
#13999=ORIENTED_EDGE('',*,*,#10646,.T.);
#14000=ORIENTED_EDGE('',*,*,#10568,.T.);
#14001=ORIENTED_EDGE('',*,*,#10647,.T.);
#14002=ORIENTED_EDGE('',*,*,#10564,.T.);
#14003=ORIENTED_EDGE('',*,*,#10648,.T.);
#14004=ORIENTED_EDGE('',*,*,#10560,.T.);
#14005=ORIENTED_EDGE('',*,*,#10649,.T.);
#14006=ORIENTED_EDGE('',*,*,#10556,.T.);
#14007=ORIENTED_EDGE('',*,*,#10650,.T.);
#14008=ORIENTED_EDGE('',*,*,#10552,.T.);
#14009=ORIENTED_EDGE('',*,*,#10651,.T.);
#14010=ORIENTED_EDGE('',*,*,#10548,.T.);
#14011=ORIENTED_EDGE('',*,*,#10652,.T.);
#14012=ORIENTED_EDGE('',*,*,#10544,.T.);
#14013=ORIENTED_EDGE('',*,*,#10653,.T.);
#14014=ORIENTED_EDGE('',*,*,#10540,.T.);
#14015=ORIENTED_EDGE('',*,*,#10654,.T.);
#14016=ORIENTED_EDGE('',*,*,#10536,.T.);
#14017=ORIENTED_EDGE('',*,*,#10655,.T.);
#14018=ORIENTED_EDGE('',*,*,#10532,.T.);
#14019=ORIENTED_EDGE('',*,*,#10656,.T.);
#14020=ORIENTED_EDGE('',*,*,#10528,.T.);
#14021=ORIENTED_EDGE('',*,*,#10657,.T.);
#14022=ORIENTED_EDGE('',*,*,#10524,.T.);
#14023=ORIENTED_EDGE('',*,*,#10658,.T.);
#14024=ORIENTED_EDGE('',*,*,#10520,.T.);
#14025=ORIENTED_EDGE('',*,*,#10659,.T.);
#14026=ORIENTED_EDGE('',*,*,#10516,.T.);
#14027=ORIENTED_EDGE('',*,*,#10660,.T.);
#14028=ORIENTED_EDGE('',*,*,#10512,.T.);
#14029=ORIENTED_EDGE('',*,*,#10661,.T.);
#14030=ORIENTED_EDGE('',*,*,#10508,.T.);
#14031=ORIENTED_EDGE('',*,*,#10662,.T.);
#14032=ORIENTED_EDGE('',*,*,#10504,.T.);
#14033=ORIENTED_EDGE('',*,*,#10663,.T.);
#14034=ORIENTED_EDGE('',*,*,#10500,.T.);
#14035=ORIENTED_EDGE('',*,*,#10664,.T.);
#14036=ORIENTED_EDGE('',*,*,#10496,.T.);
#14037=ORIENTED_EDGE('',*,*,#10665,.T.);
#14038=ORIENTED_EDGE('',*,*,#10492,.T.);
#14039=ORIENTED_EDGE('',*,*,#10666,.T.);
#14040=ORIENTED_EDGE('',*,*,#10488,.T.);
#14041=ORIENTED_EDGE('',*,*,#10667,.T.);
#14042=ORIENTED_EDGE('',*,*,#10484,.T.);
#14043=ORIENTED_EDGE('',*,*,#10668,.T.);
#14044=ORIENTED_EDGE('',*,*,#10480,.T.);
#14045=ORIENTED_EDGE('',*,*,#10669,.T.);
#14046=ORIENTED_EDGE('',*,*,#10476,.T.);
#14047=ORIENTED_EDGE('',*,*,#10670,.T.);
#14048=ORIENTED_EDGE('',*,*,#10472,.T.);
#14049=ORIENTED_EDGE('',*,*,#10671,.T.);
#14050=ORIENTED_EDGE('',*,*,#10468,.T.);
#14051=ORIENTED_EDGE('',*,*,#10672,.T.);
#14052=ORIENTED_EDGE('',*,*,#10464,.T.);
#14053=ORIENTED_EDGE('',*,*,#10673,.T.);
#14054=ORIENTED_EDGE('',*,*,#10460,.T.);
#14055=ORIENTED_EDGE('',*,*,#10674,.T.);
#14056=ORIENTED_EDGE('',*,*,#10675,.T.);
#14057=ORIENTED_EDGE('',*,*,#10455,.T.);
#14058=ORIENTED_EDGE('',*,*,#10676,.F.);
#14059=ORIENTED_EDGE('',*,*,#10677,.T.);
#14060=ORIENTED_EDGE('',*,*,#10629,.F.);
#14061=ORIENTED_EDGE('',*,*,#10625,.T.);
#14062=ORIENTED_EDGE('',*,*,#10631,.F.);
#14063=ORIENTED_EDGE('',*,*,#10678,.T.);
#14064=ORIENTED_EDGE('',*,*,#10679,.F.);
#14065=ORIENTED_EDGE('',*,*,#10621,.T.);
#14066=ORIENTED_EDGE('',*,*,#10632,.F.);
#14067=ORIENTED_EDGE('',*,*,#10627,.T.);
#14068=ORIENTED_EDGE('',*,*,#10680,.F.);
#14069=ORIENTED_EDGE('',*,*,#10617,.T.);
#14070=ORIENTED_EDGE('',*,*,#10633,.F.);
#14071=ORIENTED_EDGE('',*,*,#10623,.T.);
#14072=ORIENTED_EDGE('',*,*,#10681,.F.);
#14073=ORIENTED_EDGE('',*,*,#10613,.T.);
#14074=ORIENTED_EDGE('',*,*,#10634,.F.);
#14075=ORIENTED_EDGE('',*,*,#10619,.T.);
#14076=ORIENTED_EDGE('',*,*,#10682,.F.);
#14077=ORIENTED_EDGE('',*,*,#10609,.T.);
#14078=ORIENTED_EDGE('',*,*,#10635,.F.);
#14079=ORIENTED_EDGE('',*,*,#10615,.T.);
#14080=ORIENTED_EDGE('',*,*,#10683,.F.);
#14081=ORIENTED_EDGE('',*,*,#10605,.T.);
#14082=ORIENTED_EDGE('',*,*,#10636,.F.);
#14083=ORIENTED_EDGE('',*,*,#10611,.T.);
#14084=ORIENTED_EDGE('',*,*,#10684,.F.);
#14085=ORIENTED_EDGE('',*,*,#10601,.T.);
#14086=ORIENTED_EDGE('',*,*,#10637,.F.);
#14087=ORIENTED_EDGE('',*,*,#10607,.T.);
#14088=ORIENTED_EDGE('',*,*,#10685,.F.);
#14089=ORIENTED_EDGE('',*,*,#10597,.T.);
#14090=ORIENTED_EDGE('',*,*,#10638,.F.);
#14091=ORIENTED_EDGE('',*,*,#10603,.T.);
#14092=ORIENTED_EDGE('',*,*,#10686,.F.);
#14093=ORIENTED_EDGE('',*,*,#10593,.T.);
#14094=ORIENTED_EDGE('',*,*,#10639,.F.);
#14095=ORIENTED_EDGE('',*,*,#10599,.T.);
#14096=ORIENTED_EDGE('',*,*,#10687,.F.);
#14097=ORIENTED_EDGE('',*,*,#10589,.T.);
#14098=ORIENTED_EDGE('',*,*,#10640,.F.);
#14099=ORIENTED_EDGE('',*,*,#10595,.T.);
#14100=ORIENTED_EDGE('',*,*,#10688,.F.);
#14101=ORIENTED_EDGE('',*,*,#10585,.T.);
#14102=ORIENTED_EDGE('',*,*,#10641,.F.);
#14103=ORIENTED_EDGE('',*,*,#10591,.T.);
#14104=ORIENTED_EDGE('',*,*,#10689,.F.);
#14105=ORIENTED_EDGE('',*,*,#10581,.T.);
#14106=ORIENTED_EDGE('',*,*,#10642,.F.);
#14107=ORIENTED_EDGE('',*,*,#10587,.T.);
#14108=ORIENTED_EDGE('',*,*,#10690,.F.);
#14109=ORIENTED_EDGE('',*,*,#10577,.T.);
#14110=ORIENTED_EDGE('',*,*,#10643,.F.);
#14111=ORIENTED_EDGE('',*,*,#10583,.T.);
#14112=ORIENTED_EDGE('',*,*,#10691,.F.);
#14113=ORIENTED_EDGE('',*,*,#10573,.T.);
#14114=ORIENTED_EDGE('',*,*,#10644,.F.);
#14115=ORIENTED_EDGE('',*,*,#10579,.T.);
#14116=ORIENTED_EDGE('',*,*,#10692,.F.);
#14117=ORIENTED_EDGE('',*,*,#10569,.T.);
#14118=ORIENTED_EDGE('',*,*,#10645,.F.);
#14119=ORIENTED_EDGE('',*,*,#10575,.T.);
#14120=ORIENTED_EDGE('',*,*,#10693,.F.);
#14121=ORIENTED_EDGE('',*,*,#10565,.T.);
#14122=ORIENTED_EDGE('',*,*,#10646,.F.);
#14123=ORIENTED_EDGE('',*,*,#10571,.T.);
#14124=ORIENTED_EDGE('',*,*,#10694,.F.);
#14125=ORIENTED_EDGE('',*,*,#10561,.T.);
#14126=ORIENTED_EDGE('',*,*,#10647,.F.);
#14127=ORIENTED_EDGE('',*,*,#10567,.T.);
#14128=ORIENTED_EDGE('',*,*,#10695,.F.);
#14129=ORIENTED_EDGE('',*,*,#10557,.T.);
#14130=ORIENTED_EDGE('',*,*,#10648,.F.);
#14131=ORIENTED_EDGE('',*,*,#10563,.T.);
#14132=ORIENTED_EDGE('',*,*,#10696,.F.);
#14133=ORIENTED_EDGE('',*,*,#10553,.T.);
#14134=ORIENTED_EDGE('',*,*,#10649,.F.);
#14135=ORIENTED_EDGE('',*,*,#10559,.T.);
#14136=ORIENTED_EDGE('',*,*,#10697,.F.);
#14137=ORIENTED_EDGE('',*,*,#10549,.T.);
#14138=ORIENTED_EDGE('',*,*,#10650,.F.);
#14139=ORIENTED_EDGE('',*,*,#10555,.T.);
#14140=ORIENTED_EDGE('',*,*,#10698,.F.);
#14141=ORIENTED_EDGE('',*,*,#10545,.T.);
#14142=ORIENTED_EDGE('',*,*,#10651,.F.);
#14143=ORIENTED_EDGE('',*,*,#10551,.T.);
#14144=ORIENTED_EDGE('',*,*,#10699,.F.);
#14145=ORIENTED_EDGE('',*,*,#10541,.T.);
#14146=ORIENTED_EDGE('',*,*,#10652,.F.);
#14147=ORIENTED_EDGE('',*,*,#10547,.T.);
#14148=ORIENTED_EDGE('',*,*,#10700,.F.);
#14149=ORIENTED_EDGE('',*,*,#10537,.T.);
#14150=ORIENTED_EDGE('',*,*,#10653,.F.);
#14151=ORIENTED_EDGE('',*,*,#10543,.T.);
#14152=ORIENTED_EDGE('',*,*,#10701,.F.);
#14153=ORIENTED_EDGE('',*,*,#10533,.T.);
#14154=ORIENTED_EDGE('',*,*,#10654,.F.);
#14155=ORIENTED_EDGE('',*,*,#10539,.T.);
#14156=ORIENTED_EDGE('',*,*,#10702,.F.);
#14157=ORIENTED_EDGE('',*,*,#10529,.T.);
#14158=ORIENTED_EDGE('',*,*,#10655,.F.);
#14159=ORIENTED_EDGE('',*,*,#10535,.T.);
#14160=ORIENTED_EDGE('',*,*,#10703,.F.);
#14161=ORIENTED_EDGE('',*,*,#10525,.T.);
#14162=ORIENTED_EDGE('',*,*,#10656,.F.);
#14163=ORIENTED_EDGE('',*,*,#10531,.T.);
#14164=ORIENTED_EDGE('',*,*,#10704,.F.);
#14165=ORIENTED_EDGE('',*,*,#10521,.T.);
#14166=ORIENTED_EDGE('',*,*,#10657,.F.);
#14167=ORIENTED_EDGE('',*,*,#10527,.T.);
#14168=ORIENTED_EDGE('',*,*,#10705,.F.);
#14169=ORIENTED_EDGE('',*,*,#10517,.T.);
#14170=ORIENTED_EDGE('',*,*,#10658,.F.);
#14171=ORIENTED_EDGE('',*,*,#10523,.T.);
#14172=ORIENTED_EDGE('',*,*,#10706,.F.);
#14173=ORIENTED_EDGE('',*,*,#10513,.T.);
#14174=ORIENTED_EDGE('',*,*,#10659,.F.);
#14175=ORIENTED_EDGE('',*,*,#10519,.T.);
#14176=ORIENTED_EDGE('',*,*,#10707,.F.);
#14177=ORIENTED_EDGE('',*,*,#10509,.T.);
#14178=ORIENTED_EDGE('',*,*,#10660,.F.);
#14179=ORIENTED_EDGE('',*,*,#10515,.T.);
#14180=ORIENTED_EDGE('',*,*,#10708,.F.);
#14181=ORIENTED_EDGE('',*,*,#10505,.T.);
#14182=ORIENTED_EDGE('',*,*,#10661,.F.);
#14183=ORIENTED_EDGE('',*,*,#10511,.T.);
#14184=ORIENTED_EDGE('',*,*,#10709,.F.);
#14185=ORIENTED_EDGE('',*,*,#10501,.T.);
#14186=ORIENTED_EDGE('',*,*,#10662,.F.);
#14187=ORIENTED_EDGE('',*,*,#10507,.T.);
#14188=ORIENTED_EDGE('',*,*,#10710,.F.);
#14189=ORIENTED_EDGE('',*,*,#10497,.T.);
#14190=ORIENTED_EDGE('',*,*,#10663,.F.);
#14191=ORIENTED_EDGE('',*,*,#10503,.T.);
#14192=ORIENTED_EDGE('',*,*,#10711,.F.);
#14193=ORIENTED_EDGE('',*,*,#10493,.T.);
#14194=ORIENTED_EDGE('',*,*,#10664,.F.);
#14195=ORIENTED_EDGE('',*,*,#10499,.T.);
#14196=ORIENTED_EDGE('',*,*,#10712,.F.);
#14197=ORIENTED_EDGE('',*,*,#10489,.T.);
#14198=ORIENTED_EDGE('',*,*,#10665,.F.);
#14199=ORIENTED_EDGE('',*,*,#10495,.T.);
#14200=ORIENTED_EDGE('',*,*,#10713,.F.);
#14201=ORIENTED_EDGE('',*,*,#10485,.T.);
#14202=ORIENTED_EDGE('',*,*,#10666,.F.);
#14203=ORIENTED_EDGE('',*,*,#10491,.T.);
#14204=ORIENTED_EDGE('',*,*,#10714,.F.);
#14205=ORIENTED_EDGE('',*,*,#10481,.T.);
#14206=ORIENTED_EDGE('',*,*,#10667,.F.);
#14207=ORIENTED_EDGE('',*,*,#10487,.T.);
#14208=ORIENTED_EDGE('',*,*,#10715,.F.);
#14209=ORIENTED_EDGE('',*,*,#10477,.T.);
#14210=ORIENTED_EDGE('',*,*,#10668,.F.);
#14211=ORIENTED_EDGE('',*,*,#10483,.T.);
#14212=ORIENTED_EDGE('',*,*,#10716,.F.);
#14213=ORIENTED_EDGE('',*,*,#10473,.T.);
#14214=ORIENTED_EDGE('',*,*,#10669,.F.);
#14215=ORIENTED_EDGE('',*,*,#10479,.T.);
#14216=ORIENTED_EDGE('',*,*,#10717,.F.);
#14217=ORIENTED_EDGE('',*,*,#10469,.T.);
#14218=ORIENTED_EDGE('',*,*,#10670,.F.);
#14219=ORIENTED_EDGE('',*,*,#10475,.T.);
#14220=ORIENTED_EDGE('',*,*,#10718,.F.);
#14221=ORIENTED_EDGE('',*,*,#10465,.T.);
#14222=ORIENTED_EDGE('',*,*,#10671,.F.);
#14223=ORIENTED_EDGE('',*,*,#10471,.T.);
#14224=ORIENTED_EDGE('',*,*,#10719,.F.);
#14225=ORIENTED_EDGE('',*,*,#10461,.T.);
#14226=ORIENTED_EDGE('',*,*,#10672,.F.);
#14227=ORIENTED_EDGE('',*,*,#10467,.T.);
#14228=ORIENTED_EDGE('',*,*,#10720,.F.);
#14229=ORIENTED_EDGE('',*,*,#10457,.T.);
#14230=ORIENTED_EDGE('',*,*,#10673,.F.);
#14231=ORIENTED_EDGE('',*,*,#10463,.T.);
#14232=ORIENTED_EDGE('',*,*,#10721,.F.);
#14233=ORIENTED_EDGE('',*,*,#10677,.F.);
#14234=ORIENTED_EDGE('',*,*,#10722,.F.);
#14235=ORIENTED_EDGE('',*,*,#10678,.F.);
#14236=ORIENTED_EDGE('',*,*,#10630,.F.);
#14237=ORIENTED_EDGE('',*,*,#10454,.T.);
#14238=ORIENTED_EDGE('',*,*,#10723,.T.);
#14239=ORIENTED_EDGE('',*,*,#10458,.T.);
#14240=ORIENTED_EDGE('',*,*,#10721,.T.);
#14241=ORIENTED_EDGE('',*,*,#10462,.T.);
#14242=ORIENTED_EDGE('',*,*,#10720,.T.);
#14243=ORIENTED_EDGE('',*,*,#10466,.T.);
#14244=ORIENTED_EDGE('',*,*,#10719,.T.);
#14245=ORIENTED_EDGE('',*,*,#10470,.T.);
#14246=ORIENTED_EDGE('',*,*,#10718,.T.);
#14247=ORIENTED_EDGE('',*,*,#10474,.T.);
#14248=ORIENTED_EDGE('',*,*,#10717,.T.);
#14249=ORIENTED_EDGE('',*,*,#10478,.T.);
#14250=ORIENTED_EDGE('',*,*,#10716,.T.);
#14251=ORIENTED_EDGE('',*,*,#10482,.T.);
#14252=ORIENTED_EDGE('',*,*,#10715,.T.);
#14253=ORIENTED_EDGE('',*,*,#10486,.T.);
#14254=ORIENTED_EDGE('',*,*,#10714,.T.);
#14255=ORIENTED_EDGE('',*,*,#10490,.T.);
#14256=ORIENTED_EDGE('',*,*,#10713,.T.);
#14257=ORIENTED_EDGE('',*,*,#10494,.T.);
#14258=ORIENTED_EDGE('',*,*,#10712,.T.);
#14259=ORIENTED_EDGE('',*,*,#10498,.T.);
#14260=ORIENTED_EDGE('',*,*,#10711,.T.);
#14261=ORIENTED_EDGE('',*,*,#10502,.T.);
#14262=ORIENTED_EDGE('',*,*,#10710,.T.);
#14263=ORIENTED_EDGE('',*,*,#10506,.T.);
#14264=ORIENTED_EDGE('',*,*,#10709,.T.);
#14265=ORIENTED_EDGE('',*,*,#10510,.T.);
#14266=ORIENTED_EDGE('',*,*,#10708,.T.);
#14267=ORIENTED_EDGE('',*,*,#10514,.T.);
#14268=ORIENTED_EDGE('',*,*,#10707,.T.);
#14269=ORIENTED_EDGE('',*,*,#10518,.T.);
#14270=ORIENTED_EDGE('',*,*,#10706,.T.);
#14271=ORIENTED_EDGE('',*,*,#10522,.T.);
#14272=ORIENTED_EDGE('',*,*,#10705,.T.);
#14273=ORIENTED_EDGE('',*,*,#10526,.T.);
#14274=ORIENTED_EDGE('',*,*,#10704,.T.);
#14275=ORIENTED_EDGE('',*,*,#10530,.T.);
#14276=ORIENTED_EDGE('',*,*,#10703,.T.);
#14277=ORIENTED_EDGE('',*,*,#10534,.T.);
#14278=ORIENTED_EDGE('',*,*,#10702,.T.);
#14279=ORIENTED_EDGE('',*,*,#10538,.T.);
#14280=ORIENTED_EDGE('',*,*,#10701,.T.);
#14281=ORIENTED_EDGE('',*,*,#10542,.T.);
#14282=ORIENTED_EDGE('',*,*,#10700,.T.);
#14283=ORIENTED_EDGE('',*,*,#10546,.T.);
#14284=ORIENTED_EDGE('',*,*,#10699,.T.);
#14285=ORIENTED_EDGE('',*,*,#10550,.T.);
#14286=ORIENTED_EDGE('',*,*,#10698,.T.);
#14287=ORIENTED_EDGE('',*,*,#10554,.T.);
#14288=ORIENTED_EDGE('',*,*,#10697,.T.);
#14289=ORIENTED_EDGE('',*,*,#10558,.T.);
#14290=ORIENTED_EDGE('',*,*,#10696,.T.);
#14291=ORIENTED_EDGE('',*,*,#10562,.T.);
#14292=ORIENTED_EDGE('',*,*,#10695,.T.);
#14293=ORIENTED_EDGE('',*,*,#10566,.T.);
#14294=ORIENTED_EDGE('',*,*,#10694,.T.);
#14295=ORIENTED_EDGE('',*,*,#10570,.T.);
#14296=ORIENTED_EDGE('',*,*,#10693,.T.);
#14297=ORIENTED_EDGE('',*,*,#10574,.T.);
#14298=ORIENTED_EDGE('',*,*,#10692,.T.);
#14299=ORIENTED_EDGE('',*,*,#10578,.T.);
#14300=ORIENTED_EDGE('',*,*,#10691,.T.);
#14301=ORIENTED_EDGE('',*,*,#10582,.T.);
#14302=ORIENTED_EDGE('',*,*,#10690,.T.);
#14303=ORIENTED_EDGE('',*,*,#10586,.T.);
#14304=ORIENTED_EDGE('',*,*,#10689,.T.);
#14305=ORIENTED_EDGE('',*,*,#10590,.T.);
#14306=ORIENTED_EDGE('',*,*,#10688,.T.);
#14307=ORIENTED_EDGE('',*,*,#10594,.T.);
#14308=ORIENTED_EDGE('',*,*,#10687,.T.);
#14309=ORIENTED_EDGE('',*,*,#10598,.T.);
#14310=ORIENTED_EDGE('',*,*,#10686,.T.);
#14311=ORIENTED_EDGE('',*,*,#10602,.T.);
#14312=ORIENTED_EDGE('',*,*,#10685,.T.);
#14313=ORIENTED_EDGE('',*,*,#10606,.T.);
#14314=ORIENTED_EDGE('',*,*,#10684,.T.);
#14315=ORIENTED_EDGE('',*,*,#10610,.T.);
#14316=ORIENTED_EDGE('',*,*,#10683,.T.);
#14317=ORIENTED_EDGE('',*,*,#10614,.T.);
#14318=ORIENTED_EDGE('',*,*,#10682,.T.);
#14319=ORIENTED_EDGE('',*,*,#10618,.T.);
#14320=ORIENTED_EDGE('',*,*,#10681,.T.);
#14321=ORIENTED_EDGE('',*,*,#10622,.T.);
#14322=ORIENTED_EDGE('',*,*,#10680,.T.);
#14323=ORIENTED_EDGE('',*,*,#10626,.T.);
#14324=ORIENTED_EDGE('',*,*,#10679,.T.);
#14325=ORIENTED_EDGE('',*,*,#10722,.T.);
#14326=ORIENTED_EDGE('',*,*,#10676,.T.);
#14327=ORIENTED_EDGE('',*,*,#10724,.T.);
#14328=ORIENTED_EDGE('',*,*,#10453,.T.);
#14329=ORIENTED_EDGE('',*,*,#10674,.F.);
#14330=ORIENTED_EDGE('',*,*,#10459,.T.);
#14331=ORIENTED_EDGE('',*,*,#10723,.F.);
#14332=ORIENTED_EDGE('',*,*,#10724,.F.);
#14333=ORIENTED_EDGE('',*,*,#10725,.T.);
#14334=ORIENTED_EDGE('',*,*,#10675,.F.);
#14335=ORIENTED_EDGE('',*,*,#10725,.F.);
#14336=ORIENTED_EDGE('',*,*,#10726,.F.);
#14337=ORIENTED_EDGE('',*,*,#10727,.F.);
#14338=ORIENTED_EDGE('',*,*,#10728,.F.);
#14339=ORIENTED_EDGE('',*,*,#10729,.T.);
#14340=ORIENTED_EDGE('',*,*,#10730,.F.);
#14341=ORIENTED_EDGE('',*,*,#10729,.F.);
#14342=ORIENTED_EDGE('',*,*,#10731,.F.);
#14343=ORIENTED_EDGE('',*,*,#10732,.T.);
#14344=ORIENTED_EDGE('',*,*,#10733,.F.);
#14345=ORIENTED_EDGE('',*,*,#10734,.F.);
#14346=ORIENTED_EDGE('',*,*,#10732,.F.);
#14347=ORIENTED_EDGE('',*,*,#10735,.F.);
#14348=ORIENTED_EDGE('',*,*,#10736,.T.);
#14349=ORIENTED_EDGE('',*,*,#10737,.F.);
#14350=ORIENTED_EDGE('',*,*,#10738,.F.);
#14351=ORIENTED_EDGE('',*,*,#10739,.F.);
#14352=ORIENTED_EDGE('',*,*,#10740,.F.);
#14353=ORIENTED_EDGE('',*,*,#10741,.F.);
#14354=ORIENTED_EDGE('',*,*,#10736,.F.);
#14355=ORIENTED_EDGE('',*,*,#10742,.F.);
#14356=ORIENTED_EDGE('',*,*,#10743,.T.);
#14357=ORIENTED_EDGE('',*,*,#10744,.F.);
#14358=ORIENTED_EDGE('',*,*,#10745,.F.);
#14359=ORIENTED_EDGE('',*,*,#10743,.F.);
#14360=ORIENTED_EDGE('',*,*,#10746,.F.);
#14361=ORIENTED_EDGE('',*,*,#10747,.T.);
#14362=ORIENTED_EDGE('',*,*,#10748,.F.);
#14363=ORIENTED_EDGE('',*,*,#10747,.F.);
#14364=ORIENTED_EDGE('',*,*,#10749,.F.);
#14365=ORIENTED_EDGE('',*,*,#10750,.T.);
#14366=ORIENTED_EDGE('',*,*,#10751,.F.);
#14367=ORIENTED_EDGE('',*,*,#10752,.F.);
#14368=ORIENTED_EDGE('',*,*,#10750,.F.);
#14369=ORIENTED_EDGE('',*,*,#10753,.F.);
#14370=ORIENTED_EDGE('',*,*,#10754,.T.);
#14371=ORIENTED_EDGE('',*,*,#10755,.F.);
#14372=ORIENTED_EDGE('',*,*,#10756,.F.);
#14373=ORIENTED_EDGE('',*,*,#10757,.F.);
#14374=ORIENTED_EDGE('',*,*,#10758,.F.);
#14375=ORIENTED_EDGE('',*,*,#10759,.F.);
#14376=ORIENTED_EDGE('',*,*,#10754,.F.);
#14377=ORIENTED_EDGE('',*,*,#10760,.F.);
#14378=ORIENTED_EDGE('',*,*,#10761,.T.);
#14379=ORIENTED_EDGE('',*,*,#10762,.F.);
#14380=ORIENTED_EDGE('',*,*,#10763,.F.);
#14381=ORIENTED_EDGE('',*,*,#10761,.F.);
#14382=ORIENTED_EDGE('',*,*,#10764,.F.);
#14383=ORIENTED_EDGE('',*,*,#10765,.T.);
#14384=ORIENTED_EDGE('',*,*,#10766,.F.);
#14385=ORIENTED_EDGE('',*,*,#10765,.F.);
#14386=ORIENTED_EDGE('',*,*,#10767,.F.);
#14387=ORIENTED_EDGE('',*,*,#10768,.T.);
#14388=ORIENTED_EDGE('',*,*,#10769,.F.);
#14389=ORIENTED_EDGE('',*,*,#10770,.F.);
#14390=ORIENTED_EDGE('',*,*,#10768,.F.);
#14391=ORIENTED_EDGE('',*,*,#10771,.F.);
#14392=ORIENTED_EDGE('',*,*,#10772,.T.);
#14393=ORIENTED_EDGE('',*,*,#10773,.F.);
#14394=ORIENTED_EDGE('',*,*,#10774,.F.);
#14395=ORIENTED_EDGE('',*,*,#10775,.F.);
#14396=ORIENTED_EDGE('',*,*,#10776,.F.);
#14397=ORIENTED_EDGE('',*,*,#10777,.F.);
#14398=ORIENTED_EDGE('',*,*,#10778,.T.);
#14399=ORIENTED_EDGE('',*,*,#10779,.F.);
#14400=ORIENTED_EDGE('',*,*,#10780,.F.);
#14401=ORIENTED_EDGE('',*,*,#10781,.F.);
#14402=ORIENTED_EDGE('',*,*,#10782,.F.);
#14403=ORIENTED_EDGE('',*,*,#10783,.F.);
#14404=ORIENTED_EDGE('',*,*,#10784,.T.);
#14405=ORIENTED_EDGE('',*,*,#10785,.F.);
#14406=ORIENTED_EDGE('',*,*,#10784,.F.);
#14407=ORIENTED_EDGE('',*,*,#10786,.F.);
#14408=ORIENTED_EDGE('',*,*,#10787,.F.);
#14409=ORIENTED_EDGE('',*,*,#10788,.F.);
#14410=ORIENTED_EDGE('',*,*,#10789,.F.);
#14411=ORIENTED_EDGE('',*,*,#10790,.F.);
#14412=ORIENTED_EDGE('',*,*,#10791,.F.);
#14413=ORIENTED_EDGE('',*,*,#10792,.T.);
#14414=ORIENTED_EDGE('',*,*,#10793,.F.);
#14415=ORIENTED_EDGE('',*,*,#10794,.F.);
#14416=ORIENTED_EDGE('',*,*,#10792,.F.);
#14417=ORIENTED_EDGE('',*,*,#10795,.F.);
#14418=ORIENTED_EDGE('',*,*,#10796,.T.);
#14419=ORIENTED_EDGE('',*,*,#10797,.F.);
#14420=ORIENTED_EDGE('',*,*,#10798,.F.);
#14421=ORIENTED_EDGE('',*,*,#10799,.F.);
#14422=ORIENTED_EDGE('',*,*,#10800,.F.);
#14423=ORIENTED_EDGE('',*,*,#10801,.F.);
#14424=ORIENTED_EDGE('',*,*,#10796,.F.);
#14425=ORIENTED_EDGE('',*,*,#10802,.F.);
#14426=ORIENTED_EDGE('',*,*,#10803,.T.);
#14427=ORIENTED_EDGE('',*,*,#10804,.F.);
#14428=ORIENTED_EDGE('',*,*,#10805,.F.);
#14429=ORIENTED_EDGE('',*,*,#10803,.F.);
#14430=ORIENTED_EDGE('',*,*,#10806,.F.);
#14431=ORIENTED_EDGE('',*,*,#10727,.T.);
#14432=ORIENTED_EDGE('',*,*,#10807,.F.);
#14433=ORIENTED_EDGE('',*,*,#10808,.T.);
#14434=ORIENTED_EDGE('',*,*,#10809,.F.);
#14435=ORIENTED_EDGE('',*,*,#10810,.F.);
#14436=ORIENTED_EDGE('',*,*,#10772,.F.);
#14437=ORIENTED_EDGE('',*,*,#10811,.F.);
#14438=ORIENTED_EDGE('',*,*,#10812,.F.);
#14439=ORIENTED_EDGE('',*,*,#10813,.F.);
#14440=ORIENTED_EDGE('',*,*,#10808,.F.);
#14441=ORIENTED_EDGE('',*,*,#10814,.F.);
#14442=ORIENTED_EDGE('',*,*,#10815,.F.);
#14443=ORIENTED_EDGE('',*,*,#10816,.F.);
#14444=ORIENTED_EDGE('',*,*,#10817,.F.);
#14445=ORIENTED_EDGE('',*,*,#10778,.F.);
#14446=ORIENTED_EDGE('',*,*,#10804,.T.);
#14447=ORIENTED_EDGE('',*,*,#10726,.T.);
#14448=ORIENTED_EDGE('',*,*,#10730,.T.);
#14449=ORIENTED_EDGE('',*,*,#10818,.F.);
#14450=ORIENTED_EDGE('',*,*,#10819,.T.);
#14451=ORIENTED_EDGE('',*,*,#10820,.T.);
#14452=ORIENTED_EDGE('',*,*,#10821,.T.);
#14453=ORIENTED_EDGE('',*,*,#10739,.T.);
#14454=ORIENTED_EDGE('',*,*,#10822,.T.);
#14455=ORIENTED_EDGE('',*,*,#10820,.F.);
#14456=ORIENTED_EDGE('',*,*,#10823,.T.);
#14457=ORIENTED_EDGE('',*,*,#10744,.T.);
#14458=ORIENTED_EDGE('',*,*,#10745,.T.);
#14459=ORIENTED_EDGE('',*,*,#10748,.T.);
#14460=ORIENTED_EDGE('',*,*,#10824,.F.);
#14461=ORIENTED_EDGE('',*,*,#10737,.T.);
#14462=ORIENTED_EDGE('',*,*,#10741,.T.);
#14463=ORIENTED_EDGE('',*,*,#10824,.T.);
#14464=ORIENTED_EDGE('',*,*,#10751,.T.);
#14465=ORIENTED_EDGE('',*,*,#10752,.T.);
#14466=ORIENTED_EDGE('',*,*,#10825,.T.);
#14467=ORIENTED_EDGE('',*,*,#10826,.T.);
#14468=ORIENTED_EDGE('',*,*,#10827,.T.);
#14469=ORIENTED_EDGE('',*,*,#10828,.T.);
#14470=ORIENTED_EDGE('',*,*,#10757,.T.);
#14471=ORIENTED_EDGE('',*,*,#10829,.T.);
#14472=ORIENTED_EDGE('',*,*,#10827,.F.);
#14473=ORIENTED_EDGE('',*,*,#10830,.T.);
#14474=ORIENTED_EDGE('',*,*,#10762,.T.);
#14475=ORIENTED_EDGE('',*,*,#10763,.T.);
#14476=ORIENTED_EDGE('',*,*,#10766,.T.);
#14477=ORIENTED_EDGE('',*,*,#10831,.F.);
#14478=ORIENTED_EDGE('',*,*,#10755,.T.);
#14479=ORIENTED_EDGE('',*,*,#10759,.T.);
#14480=ORIENTED_EDGE('',*,*,#10831,.T.);
#14481=ORIENTED_EDGE('',*,*,#10769,.T.);
#14482=ORIENTED_EDGE('',*,*,#10770,.T.);
#14483=ORIENTED_EDGE('',*,*,#10832,.T.);
#14484=ORIENTED_EDGE('',*,*,#10833,.T.);
#14485=ORIENTED_EDGE('',*,*,#10834,.T.);
#14486=ORIENTED_EDGE('',*,*,#10835,.T.);
#14487=ORIENTED_EDGE('',*,*,#10775,.T.);
#14488=ORIENTED_EDGE('',*,*,#10836,.T.);
#14489=ORIENTED_EDGE('',*,*,#10834,.F.);
#14490=ORIENTED_EDGE('',*,*,#10837,.T.);
#14491=ORIENTED_EDGE('',*,*,#10773,.T.);
#14492=ORIENTED_EDGE('',*,*,#10810,.T.);
#14493=ORIENTED_EDGE('',*,*,#10838,.F.);
#14494=ORIENTED_EDGE('',*,*,#10839,.F.);
#14495=ORIENTED_EDGE('',*,*,#10840,.T.);
#14496=ORIENTED_EDGE('',*,*,#10780,.T.);
#14497=ORIENTED_EDGE('',*,*,#10841,.F.);
#14498=ORIENTED_EDGE('',*,*,#10842,.F.);
#14499=ORIENTED_EDGE('',*,*,#10843,.T.);
#14500=ORIENTED_EDGE('',*,*,#10779,.T.);
#14501=ORIENTED_EDGE('',*,*,#10817,.T.);
#14502=ORIENTED_EDGE('',*,*,#10844,.T.);
#14503=ORIENTED_EDGE('',*,*,#10845,.T.);
#14504=ORIENTED_EDGE('',*,*,#10839,.T.);
#14505=ORIENTED_EDGE('',*,*,#10846,.T.);
#14506=ORIENTED_EDGE('',*,*,#10841,.T.);
#14507=ORIENTED_EDGE('',*,*,#10788,.T.);
#14508=ORIENTED_EDGE('',*,*,#10847,.T.);
#14509=ORIENTED_EDGE('',*,*,#10848,.T.);
#14510=ORIENTED_EDGE('',*,*,#10849,.T.);
#14511=ORIENTED_EDGE('',*,*,#10798,.T.);
#14512=ORIENTED_EDGE('',*,*,#10850,.F.);
#14513=ORIENTED_EDGE('',*,*,#10740,.T.);
#14514=ORIENTED_EDGE('',*,*,#10821,.F.);
#14515=ORIENTED_EDGE('',*,*,#10822,.F.);
#14516=ORIENTED_EDGE('',*,*,#10738,.T.);
#14517=ORIENTED_EDGE('',*,*,#10825,.F.);
#14518=ORIENTED_EDGE('',*,*,#10758,.T.);
#14519=ORIENTED_EDGE('',*,*,#10828,.F.);
#14520=ORIENTED_EDGE('',*,*,#10829,.F.);
#14521=ORIENTED_EDGE('',*,*,#10756,.T.);
#14522=ORIENTED_EDGE('',*,*,#10832,.F.);
#14523=ORIENTED_EDGE('',*,*,#10776,.T.);
#14524=ORIENTED_EDGE('',*,*,#10835,.F.);
#14525=ORIENTED_EDGE('',*,*,#10836,.F.);
#14526=ORIENTED_EDGE('',*,*,#10774,.T.);
#14527=ORIENTED_EDGE('',*,*,#10840,.F.);
#14528=ORIENTED_EDGE('',*,*,#10845,.F.);
#14529=ORIENTED_EDGE('',*,*,#10851,.F.);
#14530=ORIENTED_EDGE('',*,*,#10852,.F.);
#14531=ORIENTED_EDGE('',*,*,#10853,.F.);
#14532=ORIENTED_EDGE('',*,*,#10800,.T.);
#14533=ORIENTED_EDGE('',*,*,#10854,.F.);
#14534=ORIENTED_EDGE('',*,*,#10855,.F.);
#14535=ORIENTED_EDGE('',*,*,#10856,.T.);
#14536=ORIENTED_EDGE('',*,*,#10857,.F.);
#14537=ORIENTED_EDGE('',*,*,#10858,.T.);
#14538=ORIENTED_EDGE('',*,*,#10830,.F.);
#14539=ORIENTED_EDGE('',*,*,#10826,.F.);
#14540=ORIENTED_EDGE('',*,*,#10858,.F.);
#14541=ORIENTED_EDGE('',*,*,#10859,.F.);
#14542=ORIENTED_EDGE('',*,*,#10860,.T.);
#14543=ORIENTED_EDGE('',*,*,#10837,.F.);
#14544=ORIENTED_EDGE('',*,*,#10833,.F.);
#14545=ORIENTED_EDGE('',*,*,#10860,.F.);
#14546=ORIENTED_EDGE('',*,*,#10861,.T.);
#14547=ORIENTED_EDGE('',*,*,#10862,.T.);
#14548=ORIENTED_EDGE('',*,*,#10854,.T.);
#14549=ORIENTED_EDGE('',*,*,#10799,.T.);
#14550=ORIENTED_EDGE('',*,*,#10855,.T.);
#14551=ORIENTED_EDGE('',*,*,#10862,.F.);
#14552=ORIENTED_EDGE('',*,*,#10863,.T.);
#14553=ORIENTED_EDGE('',*,*,#10864,.F.);
#14554=ORIENTED_EDGE('',*,*,#10865,.T.);
#14555=ORIENTED_EDGE('',*,*,#10863,.F.);
#14556=ORIENTED_EDGE('',*,*,#10861,.F.);
#14557=ORIENTED_EDGE('',*,*,#10865,.F.);
#14558=ORIENTED_EDGE('',*,*,#10866,.F.);
#14559=ORIENTED_EDGE('',*,*,#10867,.T.);
#14560=ORIENTED_EDGE('',*,*,#10823,.F.);
#14561=ORIENTED_EDGE('',*,*,#10819,.F.);
#14562=ORIENTED_EDGE('',*,*,#10867,.F.);
#14563=ORIENTED_EDGE('',*,*,#10868,.T.);
#14564=ORIENTED_EDGE('',*,*,#10869,.T.);
#14565=ORIENTED_EDGE('',*,*,#10870,.T.);
#14566=ORIENTED_EDGE('',*,*,#10871,.T.);
#14567=ORIENTED_EDGE('',*,*,#10790,.T.);
#14568=ORIENTED_EDGE('',*,*,#10872,.F.);
#14569=ORIENTED_EDGE('',*,*,#10873,.T.);
#14570=ORIENTED_EDGE('',*,*,#10869,.F.);
#14571=ORIENTED_EDGE('',*,*,#10874,.F.);
#14572=ORIENTED_EDGE('',*,*,#10791,.T.);
#14573=ORIENTED_EDGE('',*,*,#10874,.T.);
#14574=ORIENTED_EDGE('',*,*,#10868,.F.);
#14575=ORIENTED_EDGE('',*,*,#10875,.T.);
#14576=ORIENTED_EDGE('',*,*,#10876,.T.);
#14577=ORIENTED_EDGE('',*,*,#10877,.T.);
#14578=ORIENTED_EDGE('',*,*,#10878,.T.);
#14579=ORIENTED_EDGE('',*,*,#10879,.T.);
#14580=ORIENTED_EDGE('',*,*,#10880,.T.);
#14581=ORIENTED_EDGE('',*,*,#10881,.T.);
#14582=ORIENTED_EDGE('',*,*,#10882,.F.);
#14583=ORIENTED_EDGE('',*,*,#10883,.T.);
#14584=ORIENTED_EDGE('',*,*,#10811,.T.);
#14585=ORIENTED_EDGE('',*,*,#10807,.T.);
#14586=ORIENTED_EDGE('',*,*,#10771,.T.);
#14587=ORIENTED_EDGE('',*,*,#10767,.T.);
#14588=ORIENTED_EDGE('',*,*,#10764,.T.);
#14589=ORIENTED_EDGE('',*,*,#10760,.T.);
#14590=ORIENTED_EDGE('',*,*,#10753,.T.);
#14591=ORIENTED_EDGE('',*,*,#10749,.T.);
#14592=ORIENTED_EDGE('',*,*,#10746,.T.);
#14593=ORIENTED_EDGE('',*,*,#10742,.T.);
#14594=ORIENTED_EDGE('',*,*,#10735,.T.);
#14595=ORIENTED_EDGE('',*,*,#10731,.T.);
#14596=ORIENTED_EDGE('',*,*,#10728,.T.);
#14597=ORIENTED_EDGE('',*,*,#10806,.T.);
#14598=ORIENTED_EDGE('',*,*,#10802,.T.);
#14599=ORIENTED_EDGE('',*,*,#10795,.T.);
#14600=ORIENTED_EDGE('',*,*,#10884,.T.);
#14601=ORIENTED_EDGE('',*,*,#10885,.T.);
#14602=ORIENTED_EDGE('',*,*,#10886,.T.);
#14603=ORIENTED_EDGE('',*,*,#10887,.T.);
#14604=ORIENTED_EDGE('',*,*,#10882,.T.);
#14605=ORIENTED_EDGE('',*,*,#10888,.T.);
#14606=ORIENTED_EDGE('',*,*,#10889,.T.);
#14607=ORIENTED_EDGE('',*,*,#10890,.T.);
#14608=ORIENTED_EDGE('',*,*,#10888,.F.);
#14609=ORIENTED_EDGE('',*,*,#10881,.F.);
#14610=ORIENTED_EDGE('',*,*,#10891,.T.);
#14611=ORIENTED_EDGE('',*,*,#10892,.T.);
#14612=ORIENTED_EDGE('',*,*,#10893,.T.);
#14613=ORIENTED_EDGE('',*,*,#10894,.T.);
#14614=ORIENTED_EDGE('',*,*,#10895,.T.);
#14615=ORIENTED_EDGE('',*,*,#10896,.T.);
#14616=ORIENTED_EDGE('',*,*,#10812,.T.);
#14617=ORIENTED_EDGE('',*,*,#10883,.F.);
#14618=ORIENTED_EDGE('',*,*,#10890,.F.);
#14619=ORIENTED_EDGE('',*,*,#10897,.T.);
#14620=ORIENTED_EDGE('',*,*,#10898,.F.);
#14621=ORIENTED_EDGE('',*,*,#10787,.T.);
#14622=ORIENTED_EDGE('',*,*,#10899,.F.);
#14623=ORIENTED_EDGE('',*,*,#10900,.F.);
#14624=ORIENTED_EDGE('',*,*,#10847,.F.);
#14625=ORIENTED_EDGE('',*,*,#10816,.T.);
#14626=ORIENTED_EDGE('',*,*,#10901,.F.);
#14627=ORIENTED_EDGE('',*,*,#10902,.F.);
#14628=ORIENTED_EDGE('',*,*,#10844,.F.);
#14629=ORIENTED_EDGE('',*,*,#10815,.T.);
#14630=ORIENTED_EDGE('',*,*,#10903,.T.);
#14631=ORIENTED_EDGE('',*,*,#10904,.T.);
#14632=ORIENTED_EDGE('',*,*,#10901,.T.);
#14633=ORIENTED_EDGE('',*,*,#10900,.T.);
#14634=ORIENTED_EDGE('',*,*,#10851,.T.);
#14635=ORIENTED_EDGE('',*,*,#10902,.T.);
#14636=ORIENTED_EDGE('',*,*,#10905,.T.);
#14637=ORIENTED_EDGE('',*,*,#10783,.T.);
#14638=ORIENTED_EDGE('',*,*,#10906,.T.);
#14639=ORIENTED_EDGE('',*,*,#10907,.F.);
#14640=ORIENTED_EDGE('',*,*,#10908,.F.);
#14641=ORIENTED_EDGE('',*,*,#10852,.T.);
#14642=ORIENTED_EDGE('',*,*,#10899,.T.);
#14643=ORIENTED_EDGE('',*,*,#10786,.T.);
#14644=ORIENTED_EDGE('',*,*,#10909,.F.);
#14645=ORIENTED_EDGE('',*,*,#10910,.T.);
#14646=ORIENTED_EDGE('',*,*,#10911,.T.);
#14647=ORIENTED_EDGE('',*,*,#10912,.T.);
#14648=ORIENTED_EDGE('',*,*,#10910,.F.);
#14649=ORIENTED_EDGE('',*,*,#10913,.T.);
#14650=ORIENTED_EDGE('',*,*,#10914,.F.);
#14651=ORIENTED_EDGE('',*,*,#10915,.F.);
#14652=ORIENTED_EDGE('',*,*,#10916,.F.);
#14653=ORIENTED_EDGE('',*,*,#10917,.T.);
#14654=ORIENTED_EDGE('',*,*,#10918,.T.);
#14655=ORIENTED_EDGE('',*,*,#10914,.T.);
#14656=ORIENTED_EDGE('',*,*,#10917,.F.);
#14657=ORIENTED_EDGE('',*,*,#10919,.T.);
#14658=ORIENTED_EDGE('',*,*,#10920,.F.);
#14659=ORIENTED_EDGE('',*,*,#10921,.F.);
#14660=ORIENTED_EDGE('',*,*,#10922,.F.);
#14661=ORIENTED_EDGE('',*,*,#10923,.T.);
#14662=ORIENTED_EDGE('',*,*,#10924,.T.);
#14663=ORIENTED_EDGE('',*,*,#10920,.T.);
#14664=ORIENTED_EDGE('',*,*,#10923,.F.);
#14665=ORIENTED_EDGE('',*,*,#10925,.T.);
#14666=ORIENTED_EDGE('',*,*,#10926,.F.);
#14667=ORIENTED_EDGE('',*,*,#10927,.F.);
#14668=ORIENTED_EDGE('',*,*,#10928,.F.);
#14669=ORIENTED_EDGE('',*,*,#10929,.T.);
#14670=ORIENTED_EDGE('',*,*,#10930,.T.);
#14671=ORIENTED_EDGE('',*,*,#10926,.T.);
#14672=ORIENTED_EDGE('',*,*,#10909,.T.);
#14673=ORIENTED_EDGE('',*,*,#10931,.F.);
#14674=ORIENTED_EDGE('',*,*,#10928,.T.);
#14675=ORIENTED_EDGE('',*,*,#10925,.F.);
#14676=ORIENTED_EDGE('',*,*,#10922,.T.);
#14677=ORIENTED_EDGE('',*,*,#10919,.F.);
#14678=ORIENTED_EDGE('',*,*,#10916,.T.);
#14679=ORIENTED_EDGE('',*,*,#10913,.F.);
#14680=ORIENTED_EDGE('',*,*,#10912,.F.);
#14681=ORIENTED_EDGE('',*,*,#10932,.F.);
#14682=ORIENTED_EDGE('',*,*,#10929,.F.);
#14683=ORIENTED_EDGE('',*,*,#10931,.T.);
#14684=ORIENTED_EDGE('',*,*,#10813,.T.);
#14685=ORIENTED_EDGE('',*,*,#10898,.T.);
#14686=ORIENTED_EDGE('',*,*,#10842,.T.);
#14687=ORIENTED_EDGE('',*,*,#10846,.F.);
#14688=ORIENTED_EDGE('',*,*,#10838,.T.);
#14689=ORIENTED_EDGE('',*,*,#10809,.T.);
#14690=ORIENTED_EDGE('',*,*,#10801,.T.);
#14691=ORIENTED_EDGE('',*,*,#10853,.T.);
#14692=ORIENTED_EDGE('',*,*,#10908,.T.);
#14693=ORIENTED_EDGE('',*,*,#10933,.T.);
#14694=ORIENTED_EDGE('',*,*,#10793,.T.);
#14695=ORIENTED_EDGE('',*,*,#10934,.F.);
#14696=ORIENTED_EDGE('',*,*,#10935,.T.);
#14697=ORIENTED_EDGE('',*,*,#10856,.F.);
#14698=ORIENTED_EDGE('',*,*,#10935,.F.);
#14699=ORIENTED_EDGE('',*,*,#10782,.T.);
#14700=ORIENTED_EDGE('',*,*,#10936,.T.);
#14701=ORIENTED_EDGE('',*,*,#10937,.F.);
#14702=ORIENTED_EDGE('',*,*,#10906,.F.);
#14703=ORIENTED_EDGE('',*,*,#10904,.F.);
#14704=ORIENTED_EDGE('',*,*,#10938,.T.);
#14705=ORIENTED_EDGE('',*,*,#10848,.F.);
#14706=ORIENTED_EDGE('',*,*,#10905,.F.);
#14707=ORIENTED_EDGE('',*,*,#10939,.F.);
#14708=ORIENTED_EDGE('',*,*,#10940,.F.);
#14709=ORIENTED_EDGE('',*,*,#10941,.F.);
#14710=ORIENTED_EDGE('',*,*,#10942,.F.);
#14711=ORIENTED_EDGE('',*,*,#10943,.F.);
#14712=ORIENTED_EDGE('',*,*,#10941,.T.);
#14713=ORIENTED_EDGE('',*,*,#10944,.F.);
#14714=ORIENTED_EDGE('',*,*,#10895,.F.);
#14715=ORIENTED_EDGE('',*,*,#10945,.F.);
#14716=ORIENTED_EDGE('',*,*,#10893,.F.);
#14717=ORIENTED_EDGE('',*,*,#10894,.F.);
#14718=ORIENTED_EDGE('',*,*,#10945,.T.);
#14719=ORIENTED_EDGE('',*,*,#10946,.F.);
#14720=ORIENTED_EDGE('',*,*,#10947,.F.);
#14721=ORIENTED_EDGE('',*,*,#10948,.F.);
#14722=ORIENTED_EDGE('',*,*,#10949,.F.);
#14723=ORIENTED_EDGE('',*,*,#10950,.F.);
#14724=ORIENTED_EDGE('',*,*,#10948,.T.);
#14725=ORIENTED_EDGE('',*,*,#10871,.F.);
#14726=ORIENTED_EDGE('',*,*,#10951,.T.);
#14727=ORIENTED_EDGE('',*,*,#10942,.T.);
#14728=ORIENTED_EDGE('',*,*,#10943,.T.);
#14729=ORIENTED_EDGE('',*,*,#10940,.T.);
#14730=ORIENTED_EDGE('',*,*,#10952,.T.);
#14731=ORIENTED_EDGE('',*,*,#10953,.F.);
#14732=ORIENTED_EDGE('',*,*,#10875,.F.);
#14733=ORIENTED_EDGE('',*,*,#10949,.T.);
#14734=ORIENTED_EDGE('',*,*,#10950,.T.);
#14735=ORIENTED_EDGE('',*,*,#10947,.T.);
#14736=ORIENTED_EDGE('',*,*,#10954,.T.);
#14737=ORIENTED_EDGE('',*,*,#10955,.F.);
#14738=ORIENTED_EDGE('',*,*,#10879,.F.);
#14739=ORIENTED_EDGE('',*,*,#10956,.T.);
#14740=ORIENTED_EDGE('',*,*,#10957,.T.);
#14741=ORIENTED_EDGE('',*,*,#10958,.F.);
#14742=ORIENTED_EDGE('',*,*,#10959,.F.);
#14743=ORIENTED_EDGE('',*,*,#10960,.F.);
#14744=ORIENTED_EDGE('',*,*,#10961,.F.);
#14745=ORIENTED_EDGE('',*,*,#10962,.F.);
#14746=ORIENTED_EDGE('',*,*,#10960,.T.);
#14747=ORIENTED_EDGE('',*,*,#10961,.T.);
#14748=ORIENTED_EDGE('',*,*,#10962,.T.);
#14749=ORIENTED_EDGE('',*,*,#10959,.T.);
#14750=ORIENTED_EDGE('',*,*,#10963,.T.);
#14751=ORIENTED_EDGE('',*,*,#10964,.F.);
#14752=ORIENTED_EDGE('',*,*,#10877,.F.);
#14753=ORIENTED_EDGE('',*,*,#10965,.T.);
#14754=ORIENTED_EDGE('',*,*,#10966,.T.);
#14755=ORIENTED_EDGE('',*,*,#10805,.T.);
#14756=ORIENTED_EDGE('',*,*,#10818,.T.);
#14757=ORIENTED_EDGE('',*,*,#10733,.T.);
#14758=ORIENTED_EDGE('',*,*,#10734,.T.);
#14759=ORIENTED_EDGE('',*,*,#10850,.T.);
#14760=ORIENTED_EDGE('',*,*,#10797,.T.);
#14761=ORIENTED_EDGE('',*,*,#10967,.T.);
#14762=ORIENTED_EDGE('',*,*,#10968,.T.);
#14763=ORIENTED_EDGE('',*,*,#10969,.T.);
#14764=ORIENTED_EDGE('',*,*,#10968,.F.);
#14765=ORIENTED_EDGE('',*,*,#10969,.F.);
#14766=ORIENTED_EDGE('',*,*,#10970,.F.);
#14767=ORIENTED_EDGE('',*,*,#10971,.T.);
#14768=ORIENTED_EDGE('',*,*,#10972,.T.);
#14769=ORIENTED_EDGE('',*,*,#10967,.F.);
#14770=ORIENTED_EDGE('',*,*,#10972,.F.);
#14771=ORIENTED_EDGE('',*,*,#10973,.T.);
#14772=ORIENTED_EDGE('',*,*,#10974,.T.);
#14773=ORIENTED_EDGE('',*,*,#10970,.T.);
#14774=ORIENTED_EDGE('',*,*,#10974,.F.);
#14775=ORIENTED_EDGE('',*,*,#10975,.T.);
#14776=ORIENTED_EDGE('',*,*,#10973,.F.);
#14777=ORIENTED_EDGE('',*,*,#10976,.T.);
#14778=ORIENTED_EDGE('',*,*,#10977,.T.);
#14779=ORIENTED_EDGE('',*,*,#10976,.F.);
#14780=ORIENTED_EDGE('',*,*,#10975,.F.);
#14781=ORIENTED_EDGE('',*,*,#10859,.T.);
#14782=ORIENTED_EDGE('',*,*,#10978,.F.);
#14783=ORIENTED_EDGE('',*,*,#10884,.F.);
#14784=ORIENTED_EDGE('',*,*,#10979,.T.);
#14785=ORIENTED_EDGE('',*,*,#10978,.T.);
#14786=ORIENTED_EDGE('',*,*,#10979,.F.);
#14787=ORIENTED_EDGE('',*,*,#10866,.T.);
#14788=ORIENTED_EDGE('',*,*,#10980,.F.);
#14789=ORIENTED_EDGE('',*,*,#10885,.F.);
#14790=ORIENTED_EDGE('',*,*,#10981,.T.);
#14791=ORIENTED_EDGE('',*,*,#10980,.T.);
#14792=ORIENTED_EDGE('',*,*,#10981,.F.);
#14793=ORIENTED_EDGE('',*,*,#10864,.T.);
#14794=ORIENTED_EDGE('',*,*,#10982,.F.);
#14795=ORIENTED_EDGE('',*,*,#10886,.F.);
#14796=ORIENTED_EDGE('',*,*,#10983,.T.);
#14797=ORIENTED_EDGE('',*,*,#10982,.T.);
#14798=ORIENTED_EDGE('',*,*,#10983,.F.);
#14799=ORIENTED_EDGE('',*,*,#10857,.T.);
#14800=ORIENTED_EDGE('',*,*,#10984,.F.);
#14801=ORIENTED_EDGE('',*,*,#10887,.F.);
#14802=ORIENTED_EDGE('',*,*,#10985,.T.);
#14803=ORIENTED_EDGE('',*,*,#10984,.T.);
#14804=ORIENTED_EDGE('',*,*,#10985,.F.);
#14805=ORIENTED_EDGE('',*,*,#10777,.T.);
#14806=ORIENTED_EDGE('',*,*,#10843,.F.);
#14807=ORIENTED_EDGE('',*,*,#10897,.F.);
#14808=ORIENTED_EDGE('',*,*,#10889,.F.);
#14809=ORIENTED_EDGE('',*,*,#10896,.F.);
#14810=ORIENTED_EDGE('',*,*,#10944,.T.);
#14811=ORIENTED_EDGE('',*,*,#10892,.F.);
#14812=ORIENTED_EDGE('',*,*,#10986,.F.);
#14813=ORIENTED_EDGE('',*,*,#10954,.F.);
#14814=ORIENTED_EDGE('',*,*,#10946,.T.);
#14815=ORIENTED_EDGE('',*,*,#10957,.F.);
#14816=ORIENTED_EDGE('',*,*,#10987,.F.);
#14817=ORIENTED_EDGE('',*,*,#10963,.F.);
#14818=ORIENTED_EDGE('',*,*,#10958,.T.);
#14819=ORIENTED_EDGE('',*,*,#10966,.F.);
#14820=ORIENTED_EDGE('',*,*,#10988,.F.);
#14821=ORIENTED_EDGE('',*,*,#10952,.F.);
#14822=ORIENTED_EDGE('',*,*,#10939,.T.);
#14823=ORIENTED_EDGE('',*,*,#10951,.F.);
#14824=ORIENTED_EDGE('',*,*,#10870,.F.);
#14825=ORIENTED_EDGE('',*,*,#10873,.F.);
#14826=ORIENTED_EDGE('',*,*,#10936,.F.);
#14827=ORIENTED_EDGE('',*,*,#10781,.T.);
#14828=ORIENTED_EDGE('',*,*,#10785,.T.);
#14829=ORIENTED_EDGE('',*,*,#10849,.F.);
#14830=ORIENTED_EDGE('',*,*,#10938,.F.);
#14831=ORIENTED_EDGE('',*,*,#10903,.F.);
#14832=ORIENTED_EDGE('',*,*,#10814,.T.);
#14833=ORIENTED_EDGE('',*,*,#10927,.T.);
#14834=ORIENTED_EDGE('',*,*,#10930,.F.);
#14835=ORIENTED_EDGE('',*,*,#10932,.T.);
#14836=ORIENTED_EDGE('',*,*,#10911,.F.);
#14837=ORIENTED_EDGE('',*,*,#10915,.T.);
#14838=ORIENTED_EDGE('',*,*,#10918,.F.);
#14839=ORIENTED_EDGE('',*,*,#10921,.T.);
#14840=ORIENTED_EDGE('',*,*,#10924,.F.);
#14841=ORIENTED_EDGE('',*,*,#10971,.F.);
#14842=ORIENTED_EDGE('',*,*,#10989,.F.);
#14843=ORIENTED_EDGE('',*,*,#10990,.T.);
#14844=ORIENTED_EDGE('',*,*,#10991,.T.);
#14845=ORIENTED_EDGE('',*,*,#10990,.F.);
#14846=ORIENTED_EDGE('',*,*,#10991,.F.);
#14847=ORIENTED_EDGE('',*,*,#10934,.T.);
#14848=ORIENTED_EDGE('',*,*,#10977,.F.);
#14849=ORIENTED_EDGE('',*,*,#10989,.T.);
#14850=ORIENTED_EDGE('',*,*,#10880,.F.);
#14851=ORIENTED_EDGE('',*,*,#10955,.T.);
#14852=ORIENTED_EDGE('',*,*,#10986,.T.);
#14853=ORIENTED_EDGE('',*,*,#10891,.F.);
#14854=ORIENTED_EDGE('',*,*,#10878,.F.);
#14855=ORIENTED_EDGE('',*,*,#10964,.T.);
#14856=ORIENTED_EDGE('',*,*,#10987,.T.);
#14857=ORIENTED_EDGE('',*,*,#10956,.F.);
#14858=ORIENTED_EDGE('',*,*,#10876,.F.);
#14859=ORIENTED_EDGE('',*,*,#10953,.T.);
#14860=ORIENTED_EDGE('',*,*,#10988,.T.);
#14861=ORIENTED_EDGE('',*,*,#10965,.F.);
#14862=ORIENTED_EDGE('',*,*,#10794,.T.);
#14863=ORIENTED_EDGE('',*,*,#10933,.F.);
#14864=ORIENTED_EDGE('',*,*,#10907,.T.);
#14865=ORIENTED_EDGE('',*,*,#10937,.T.);
#14866=ORIENTED_EDGE('',*,*,#10872,.T.);
#14867=ORIENTED_EDGE('',*,*,#10789,.T.);
#14868=ORIENTED_EDGE('',*,*,#10992,.T.);
#14869=ORIENTED_EDGE('',*,*,#10993,.T.);
#14870=ORIENTED_EDGE('',*,*,#10994,.T.);
#14871=ORIENTED_EDGE('',*,*,#10995,.T.);
#14872=ORIENTED_EDGE('',*,*,#10993,.F.);
#14873=ORIENTED_EDGE('',*,*,#10995,.F.);
#14874=ORIENTED_EDGE('',*,*,#10996,.T.);
#14875=ORIENTED_EDGE('',*,*,#10997,.F.);
#14876=ORIENTED_EDGE('',*,*,#10998,.F.);
#14877=ORIENTED_EDGE('',*,*,#10996,.F.);
#14878=ORIENTED_EDGE('',*,*,#10994,.F.);
#14879=ORIENTED_EDGE('',*,*,#10992,.F.);
#14880=ORIENTED_EDGE('',*,*,#10999,.F.);
#14881=ORIENTED_EDGE('',*,*,#10998,.T.);
#14882=ORIENTED_EDGE('',*,*,#11000,.T.);
#14883=ORIENTED_EDGE('',*,*,#11001,.T.);
#14884=ORIENTED_EDGE('',*,*,#11000,.F.);
#14885=ORIENTED_EDGE('',*,*,#10997,.T.);
#14886=ORIENTED_EDGE('',*,*,#11001,.F.);
#14887=ORIENTED_EDGE('',*,*,#11002,.T.);
#14888=ORIENTED_EDGE('',*,*,#11002,.F.);
#14889=ORIENTED_EDGE('',*,*,#11003,.T.);
#14890=ORIENTED_EDGE('',*,*,#10999,.T.);
#14891=ORIENTED_EDGE('',*,*,#11003,.F.);
#14892=ORIENTED_EDGE('',*,*,#11004,.T.);
#14893=ORIENTED_EDGE('',*,*,#11005,.F.);
#14894=ORIENTED_EDGE('',*,*,#11006,.T.);
#14895=ORIENTED_EDGE('',*,*,#11007,.F.);
#14896=ORIENTED_EDGE('',*,*,#11006,.F.);
#14897=ORIENTED_EDGE('',*,*,#11008,.F.);
#14898=ORIENTED_EDGE('',*,*,#11009,.F.);
#14899=ORIENTED_EDGE('',*,*,#11010,.F.);
#14900=ORIENTED_EDGE('',*,*,#11011,.F.);
#14901=ORIENTED_EDGE('',*,*,#11012,.T.);
#14902=ORIENTED_EDGE('',*,*,#11013,.T.);
#14903=ORIENTED_EDGE('',*,*,#11014,.F.);
#14904=ORIENTED_EDGE('',*,*,#11013,.F.);
#14905=ORIENTED_EDGE('',*,*,#11015,.T.);
#14906=ORIENTED_EDGE('',*,*,#11009,.T.);
#14907=ORIENTED_EDGE('',*,*,#11016,.F.);
#14908=ORIENTED_EDGE('',*,*,#11017,.F.);
#14909=ORIENTED_EDGE('',*,*,#11018,.F.);
#14910=ORIENTED_EDGE('',*,*,#11019,.F.);
#14911=ORIENTED_EDGE('',*,*,#11007,.T.);
#14912=ORIENTED_EDGE('',*,*,#11010,.T.);
#14913=ORIENTED_EDGE('',*,*,#11015,.F.);
#14914=ORIENTED_EDGE('',*,*,#11012,.F.);
#14915=ORIENTED_EDGE('',*,*,#11019,.T.);
#14916=ORIENTED_EDGE('',*,*,#11020,.F.);
#14917=ORIENTED_EDGE('',*,*,#11021,.F.);
#14918=ORIENTED_EDGE('',*,*,#11004,.F.);
#14919=ORIENTED_EDGE('',*,*,#11021,.T.);
#14920=ORIENTED_EDGE('',*,*,#11022,.F.);
#14921=ORIENTED_EDGE('',*,*,#11023,.F.);
#14922=ORIENTED_EDGE('',*,*,#11014,.T.);
#14923=ORIENTED_EDGE('',*,*,#11016,.T.);
#14924=ORIENTED_EDGE('',*,*,#11008,.T.);
#14925=ORIENTED_EDGE('',*,*,#11005,.T.);
#14926=ORIENTED_EDGE('',*,*,#11023,.T.);
#14927=ORIENTED_EDGE('',*,*,#11024,.F.);
#14928=ORIENTED_EDGE('',*,*,#11017,.T.);
#14929=ORIENTED_EDGE('',*,*,#11011,.T.);
#14930=ORIENTED_EDGE('',*,*,#11024,.T.);
#14931=ORIENTED_EDGE('',*,*,#11022,.T.);
#14932=ORIENTED_EDGE('',*,*,#11020,.T.);
#14933=ORIENTED_EDGE('',*,*,#11018,.T.);
#14934=ORIENTED_EDGE('',*,*,#11025,.F.);
#14935=ORIENTED_EDGE('',*,*,#11026,.T.);
#14936=ORIENTED_EDGE('',*,*,#11027,.T.);
#14937=ORIENTED_EDGE('',*,*,#11028,.F.);
#14938=ORIENTED_EDGE('',*,*,#11029,.T.);
#14939=ORIENTED_EDGE('',*,*,#11028,.T.);
#14940=ORIENTED_EDGE('',*,*,#11030,.T.);
#14941=ORIENTED_EDGE('',*,*,#11031,.F.);
#14942=ORIENTED_EDGE('',*,*,#11032,.T.);
#14943=ORIENTED_EDGE('',*,*,#11033,.F.);
#14944=ORIENTED_EDGE('',*,*,#11034,.F.);
#14945=ORIENTED_EDGE('',*,*,#11035,.F.);
#14946=ORIENTED_EDGE('',*,*,#11036,.T.);
#14947=ORIENTED_EDGE('',*,*,#11025,.T.);
#14948=ORIENTED_EDGE('',*,*,#11029,.F.);
#14949=ORIENTED_EDGE('',*,*,#11037,.T.);
#14950=ORIENTED_EDGE('',*,*,#11038,.T.);
#14951=ORIENTED_EDGE('',*,*,#11026,.F.);
#14952=ORIENTED_EDGE('',*,*,#11036,.F.);
#14953=ORIENTED_EDGE('',*,*,#11039,.F.);
#14954=ORIENTED_EDGE('',*,*,#11040,.F.);
#14955=ORIENTED_EDGE('',*,*,#11041,.F.);
#14956=ORIENTED_EDGE('',*,*,#11042,.F.);
#14957=ORIENTED_EDGE('',*,*,#11030,.F.);
#14958=ORIENTED_EDGE('',*,*,#11027,.F.);
#14959=ORIENTED_EDGE('',*,*,#11038,.F.);
#14960=ORIENTED_EDGE('',*,*,#11043,.T.);
#14961=ORIENTED_EDGE('',*,*,#11031,.T.);
#14962=ORIENTED_EDGE('',*,*,#11042,.T.);
#14963=ORIENTED_EDGE('',*,*,#11037,.F.);
#14964=ORIENTED_EDGE('',*,*,#11041,.T.);
#14965=ORIENTED_EDGE('',*,*,#11044,.F.);
#14966=ORIENTED_EDGE('',*,*,#11032,.F.);
#14967=ORIENTED_EDGE('',*,*,#11043,.F.);
#14968=ORIENTED_EDGE('',*,*,#11034,.T.);
#14969=ORIENTED_EDGE('',*,*,#11045,.F.);
#14970=ORIENTED_EDGE('',*,*,#11039,.T.);
#14971=ORIENTED_EDGE('',*,*,#11035,.T.);
#14972=ORIENTED_EDGE('',*,*,#11045,.T.);
#14973=ORIENTED_EDGE('',*,*,#11033,.T.);
#14974=ORIENTED_EDGE('',*,*,#11044,.T.);
#14975=ORIENTED_EDGE('',*,*,#11040,.T.);
#14976=ORIENTED_EDGE('',*,*,#11046,.T.);
#14977=ORIENTED_EDGE('',*,*,#11047,.F.);
#14978=ORIENTED_EDGE('',*,*,#11048,.T.);
#14979=ORIENTED_EDGE('',*,*,#11049,.T.);
#14980=ORIENTED_EDGE('',*,*,#11050,.T.);
#14981=ORIENTED_EDGE('',*,*,#11051,.F.);
#14982=ORIENTED_EDGE('',*,*,#11052,.T.);
#14983=ORIENTED_EDGE('',*,*,#11047,.T.);
#14984=ORIENTED_EDGE('',*,*,#11053,.T.);
#14985=ORIENTED_EDGE('',*,*,#11054,.F.);
#14986=ORIENTED_EDGE('',*,*,#11055,.T.);
#14987=ORIENTED_EDGE('',*,*,#11051,.T.);
#14988=ORIENTED_EDGE('',*,*,#11056,.T.);
#14989=ORIENTED_EDGE('',*,*,#11057,.F.);
#14990=ORIENTED_EDGE('',*,*,#11058,.T.);
#14991=ORIENTED_EDGE('',*,*,#11054,.T.);
#14992=ORIENTED_EDGE('',*,*,#11059,.T.);
#14993=ORIENTED_EDGE('',*,*,#11060,.F.);
#14994=ORIENTED_EDGE('',*,*,#11061,.T.);
#14995=ORIENTED_EDGE('',*,*,#11057,.T.);
#14996=ORIENTED_EDGE('',*,*,#11062,.T.);
#14997=ORIENTED_EDGE('',*,*,#11063,.F.);
#14998=ORIENTED_EDGE('',*,*,#11064,.T.);
#14999=ORIENTED_EDGE('',*,*,#11060,.T.);
#15000=ORIENTED_EDGE('',*,*,#11065,.T.);
#15001=ORIENTED_EDGE('',*,*,#11066,.F.);
#15002=ORIENTED_EDGE('',*,*,#11067,.T.);
#15003=ORIENTED_EDGE('',*,*,#11063,.T.);
#15004=ORIENTED_EDGE('',*,*,#11068,.T.);
#15005=ORIENTED_EDGE('',*,*,#11069,.F.);
#15006=ORIENTED_EDGE('',*,*,#11070,.T.);
#15007=ORIENTED_EDGE('',*,*,#11066,.T.);
#15008=ORIENTED_EDGE('',*,*,#11071,.T.);
#15009=ORIENTED_EDGE('',*,*,#11072,.F.);
#15010=ORIENTED_EDGE('',*,*,#11073,.T.);
#15011=ORIENTED_EDGE('',*,*,#11069,.T.);
#15012=ORIENTED_EDGE('',*,*,#11074,.T.);
#15013=ORIENTED_EDGE('',*,*,#11075,.F.);
#15014=ORIENTED_EDGE('',*,*,#11076,.T.);
#15015=ORIENTED_EDGE('',*,*,#11072,.T.);
#15016=ORIENTED_EDGE('',*,*,#11077,.T.);
#15017=ORIENTED_EDGE('',*,*,#11078,.F.);
#15018=ORIENTED_EDGE('',*,*,#11079,.T.);
#15019=ORIENTED_EDGE('',*,*,#11075,.T.);
#15020=ORIENTED_EDGE('',*,*,#11080,.T.);
#15021=ORIENTED_EDGE('',*,*,#11081,.F.);
#15022=ORIENTED_EDGE('',*,*,#11082,.T.);
#15023=ORIENTED_EDGE('',*,*,#11078,.T.);
#15024=ORIENTED_EDGE('',*,*,#11083,.T.);
#15025=ORIENTED_EDGE('',*,*,#11084,.F.);
#15026=ORIENTED_EDGE('',*,*,#11085,.T.);
#15027=ORIENTED_EDGE('',*,*,#11081,.T.);
#15028=ORIENTED_EDGE('',*,*,#11086,.T.);
#15029=ORIENTED_EDGE('',*,*,#11087,.F.);
#15030=ORIENTED_EDGE('',*,*,#11088,.T.);
#15031=ORIENTED_EDGE('',*,*,#11084,.T.);
#15032=ORIENTED_EDGE('',*,*,#11089,.T.);
#15033=ORIENTED_EDGE('',*,*,#11090,.F.);
#15034=ORIENTED_EDGE('',*,*,#11091,.T.);
#15035=ORIENTED_EDGE('',*,*,#11087,.T.);
#15036=ORIENTED_EDGE('',*,*,#11092,.T.);
#15037=ORIENTED_EDGE('',*,*,#11093,.F.);
#15038=ORIENTED_EDGE('',*,*,#11094,.T.);
#15039=ORIENTED_EDGE('',*,*,#11090,.T.);
#15040=ORIENTED_EDGE('',*,*,#11095,.T.);
#15041=ORIENTED_EDGE('',*,*,#11096,.F.);
#15042=ORIENTED_EDGE('',*,*,#11097,.T.);
#15043=ORIENTED_EDGE('',*,*,#11093,.T.);
#15044=ORIENTED_EDGE('',*,*,#11098,.T.);
#15045=ORIENTED_EDGE('',*,*,#11099,.F.);
#15046=ORIENTED_EDGE('',*,*,#11100,.T.);
#15047=ORIENTED_EDGE('',*,*,#11096,.T.);
#15048=ORIENTED_EDGE('',*,*,#11101,.T.);
#15049=ORIENTED_EDGE('',*,*,#11102,.F.);
#15050=ORIENTED_EDGE('',*,*,#11103,.T.);
#15051=ORIENTED_EDGE('',*,*,#11099,.T.);
#15052=ORIENTED_EDGE('',*,*,#11104,.T.);
#15053=ORIENTED_EDGE('',*,*,#11049,.F.);
#15054=ORIENTED_EDGE('',*,*,#11105,.T.);
#15055=ORIENTED_EDGE('',*,*,#11102,.T.);
#15056=ORIENTED_EDGE('',*,*,#11048,.F.);
#15057=ORIENTED_EDGE('',*,*,#11052,.F.);
#15058=ORIENTED_EDGE('',*,*,#11055,.F.);
#15059=ORIENTED_EDGE('',*,*,#11058,.F.);
#15060=ORIENTED_EDGE('',*,*,#11061,.F.);
#15061=ORIENTED_EDGE('',*,*,#11064,.F.);
#15062=ORIENTED_EDGE('',*,*,#11067,.F.);
#15063=ORIENTED_EDGE('',*,*,#11070,.F.);
#15064=ORIENTED_EDGE('',*,*,#11073,.F.);
#15065=ORIENTED_EDGE('',*,*,#11076,.F.);
#15066=ORIENTED_EDGE('',*,*,#11079,.F.);
#15067=ORIENTED_EDGE('',*,*,#11082,.F.);
#15068=ORIENTED_EDGE('',*,*,#11085,.F.);
#15069=ORIENTED_EDGE('',*,*,#11088,.F.);
#15070=ORIENTED_EDGE('',*,*,#11091,.F.);
#15071=ORIENTED_EDGE('',*,*,#11094,.F.);
#15072=ORIENTED_EDGE('',*,*,#11097,.F.);
#15073=ORIENTED_EDGE('',*,*,#11100,.F.);
#15074=ORIENTED_EDGE('',*,*,#11103,.F.);
#15075=ORIENTED_EDGE('',*,*,#11105,.F.);
#15076=ORIENTED_EDGE('',*,*,#11046,.F.);
#15077=ORIENTED_EDGE('',*,*,#11104,.F.);
#15078=ORIENTED_EDGE('',*,*,#11101,.F.);
#15079=ORIENTED_EDGE('',*,*,#11098,.F.);
#15080=ORIENTED_EDGE('',*,*,#11095,.F.);
#15081=ORIENTED_EDGE('',*,*,#11092,.F.);
#15082=ORIENTED_EDGE('',*,*,#11089,.F.);
#15083=ORIENTED_EDGE('',*,*,#11086,.F.);
#15084=ORIENTED_EDGE('',*,*,#11083,.F.);
#15085=ORIENTED_EDGE('',*,*,#11080,.F.);
#15086=ORIENTED_EDGE('',*,*,#11077,.F.);
#15087=ORIENTED_EDGE('',*,*,#11074,.F.);
#15088=ORIENTED_EDGE('',*,*,#11071,.F.);
#15089=ORIENTED_EDGE('',*,*,#11068,.F.);
#15090=ORIENTED_EDGE('',*,*,#11065,.F.);
#15091=ORIENTED_EDGE('',*,*,#11062,.F.);
#15092=ORIENTED_EDGE('',*,*,#11059,.F.);
#15093=ORIENTED_EDGE('',*,*,#11056,.F.);
#15094=ORIENTED_EDGE('',*,*,#11053,.F.);
#15095=ORIENTED_EDGE('',*,*,#11050,.F.);
#15096=ORIENTED_EDGE('',*,*,#11106,.T.);
#15097=ORIENTED_EDGE('',*,*,#11107,.T.);
#15098=ORIENTED_EDGE('',*,*,#11108,.T.);
#15099=ORIENTED_EDGE('',*,*,#11109,.T.);
#15100=ORIENTED_EDGE('',*,*,#11107,.F.);
#15101=ORIENTED_EDGE('',*,*,#11110,.F.);
#15102=ORIENTED_EDGE('',*,*,#11111,.F.);
#15103=ORIENTED_EDGE('',*,*,#11112,.F.);
#15104=ORIENTED_EDGE('',*,*,#11113,.T.);
#15105=ORIENTED_EDGE('',*,*,#11114,.T.);
#15106=ORIENTED_EDGE('',*,*,#11115,.T.);
#15107=ORIENTED_EDGE('',*,*,#11111,.T.);
#15108=ORIENTED_EDGE('',*,*,#11114,.F.);
#15109=ORIENTED_EDGE('',*,*,#11116,.F.);
#15110=ORIENTED_EDGE('',*,*,#11117,.F.);
#15111=ORIENTED_EDGE('',*,*,#11118,.F.);
#15112=ORIENTED_EDGE('',*,*,#11119,.T.);
#15113=ORIENTED_EDGE('',*,*,#11120,.T.);
#15114=ORIENTED_EDGE('',*,*,#11121,.T.);
#15115=ORIENTED_EDGE('',*,*,#11122,.T.);
#15116=ORIENTED_EDGE('',*,*,#11120,.F.);
#15117=ORIENTED_EDGE('',*,*,#11123,.F.);
#15118=ORIENTED_EDGE('',*,*,#11124,.F.);
#15119=ORIENTED_EDGE('',*,*,#11125,.F.);
#15120=ORIENTED_EDGE('',*,*,#11126,.T.);
#15121=ORIENTED_EDGE('',*,*,#11127,.T.);
#15122=ORIENTED_EDGE('',*,*,#11128,.T.);
#15123=ORIENTED_EDGE('',*,*,#11124,.T.);
#15124=ORIENTED_EDGE('',*,*,#11127,.F.);
#15125=ORIENTED_EDGE('',*,*,#11129,.F.);
#15126=ORIENTED_EDGE('',*,*,#11130,.F.);
#15127=ORIENTED_EDGE('',*,*,#11131,.F.);
#15128=ORIENTED_EDGE('',*,*,#11132,.T.);
#15129=ORIENTED_EDGE('',*,*,#11133,.T.);
#15130=ORIENTED_EDGE('',*,*,#11134,.T.);
#15131=ORIENTED_EDGE('',*,*,#11135,.T.);
#15132=ORIENTED_EDGE('',*,*,#11133,.F.);
#15133=ORIENTED_EDGE('',*,*,#11136,.F.);
#15134=ORIENTED_EDGE('',*,*,#11137,.F.);
#15135=ORIENTED_EDGE('',*,*,#11138,.F.);
#15136=ORIENTED_EDGE('',*,*,#11139,.T.);
#15137=ORIENTED_EDGE('',*,*,#11140,.T.);
#15138=ORIENTED_EDGE('',*,*,#11141,.T.);
#15139=ORIENTED_EDGE('',*,*,#11137,.T.);
#15140=ORIENTED_EDGE('',*,*,#11140,.F.);
#15141=ORIENTED_EDGE('',*,*,#11142,.F.);
#15142=ORIENTED_EDGE('',*,*,#11143,.F.);
#15143=ORIENTED_EDGE('',*,*,#11144,.F.);
#15144=ORIENTED_EDGE('',*,*,#11145,.T.);
#15145=ORIENTED_EDGE('',*,*,#11146,.T.);
#15146=ORIENTED_EDGE('',*,*,#11147,.T.);
#15147=ORIENTED_EDGE('',*,*,#11148,.T.);
#15148=ORIENTED_EDGE('',*,*,#11146,.F.);
#15149=ORIENTED_EDGE('',*,*,#11149,.F.);
#15150=ORIENTED_EDGE('',*,*,#11150,.F.);
#15151=ORIENTED_EDGE('',*,*,#11151,.F.);
#15152=ORIENTED_EDGE('',*,*,#11152,.T.);
#15153=ORIENTED_EDGE('',*,*,#11153,.T.);
#15154=ORIENTED_EDGE('',*,*,#11154,.T.);
#15155=ORIENTED_EDGE('',*,*,#11150,.T.);
#15156=ORIENTED_EDGE('',*,*,#11153,.F.);
#15157=ORIENTED_EDGE('',*,*,#11155,.F.);
#15158=ORIENTED_EDGE('',*,*,#11156,.F.);
#15159=ORIENTED_EDGE('',*,*,#11157,.F.);
#15160=ORIENTED_EDGE('',*,*,#11158,.T.);
#15161=ORIENTED_EDGE('',*,*,#11159,.T.);
#15162=ORIENTED_EDGE('',*,*,#11160,.T.);
#15163=ORIENTED_EDGE('',*,*,#11161,.T.);
#15164=ORIENTED_EDGE('',*,*,#11159,.F.);
#15165=ORIENTED_EDGE('',*,*,#11162,.F.);
#15166=ORIENTED_EDGE('',*,*,#11163,.F.);
#15167=ORIENTED_EDGE('',*,*,#11164,.F.);
#15168=ORIENTED_EDGE('',*,*,#11165,.T.);
#15169=ORIENTED_EDGE('',*,*,#11166,.T.);
#15170=ORIENTED_EDGE('',*,*,#11167,.T.);
#15171=ORIENTED_EDGE('',*,*,#11163,.T.);
#15172=ORIENTED_EDGE('',*,*,#11166,.F.);
#15173=ORIENTED_EDGE('',*,*,#11168,.F.);
#15174=ORIENTED_EDGE('',*,*,#11169,.F.);
#15175=ORIENTED_EDGE('',*,*,#11170,.F.);
#15176=ORIENTED_EDGE('',*,*,#11161,.F.);
#15177=ORIENTED_EDGE('',*,*,#11171,.F.);
#15178=ORIENTED_EDGE('',*,*,#11172,.F.);
#15179=ORIENTED_EDGE('',*,*,#11173,.F.);
#15180=ORIENTED_EDGE('',*,*,#11148,.F.);
#15181=ORIENTED_EDGE('',*,*,#11174,.F.);
#15182=ORIENTED_EDGE('',*,*,#11175,.F.);
#15183=ORIENTED_EDGE('',*,*,#11176,.F.);
#15184=ORIENTED_EDGE('',*,*,#11122,.F.);
#15185=ORIENTED_EDGE('',*,*,#11177,.F.);
#15186=ORIENTED_EDGE('',*,*,#11178,.F.);
#15187=ORIENTED_EDGE('',*,*,#11179,.F.);
#15188=ORIENTED_EDGE('',*,*,#11109,.F.);
#15189=ORIENTED_EDGE('',*,*,#11180,.F.);
#15190=ORIENTED_EDGE('',*,*,#11181,.F.);
#15191=ORIENTED_EDGE('',*,*,#11182,.F.);
#15192=ORIENTED_EDGE('',*,*,#11169,.T.);
#15193=ORIENTED_EDGE('',*,*,#11183,.F.);
#15194=ORIENTED_EDGE('',*,*,#11184,.T.);
#15195=ORIENTED_EDGE('',*,*,#11185,.F.);
#15196=ORIENTED_EDGE('',*,*,#11175,.T.);
#15197=ORIENTED_EDGE('',*,*,#11186,.F.);
#15198=ORIENTED_EDGE('',*,*,#11143,.T.);
#15199=ORIENTED_EDGE('',*,*,#11187,.F.);
#15200=ORIENTED_EDGE('',*,*,#11171,.T.);
#15201=ORIENTED_EDGE('',*,*,#11160,.F.);
#15202=ORIENTED_EDGE('',*,*,#11164,.T.);
#15203=ORIENTED_EDGE('',*,*,#11167,.F.);
#15204=ORIENTED_EDGE('',*,*,#11170,.T.);
#15205=ORIENTED_EDGE('',*,*,#11185,.T.);
#15206=ORIENTED_EDGE('',*,*,#11188,.T.);
#15207=ORIENTED_EDGE('',*,*,#11189,.T.);
#15208=ORIENTED_EDGE('',*,*,#11190,.T.);
#15209=ORIENTED_EDGE('',*,*,#11191,.T.);
#15210=ORIENTED_EDGE('',*,*,#11180,.T.);
#15211=ORIENTED_EDGE('',*,*,#11108,.F.);
#15212=ORIENTED_EDGE('',*,*,#11112,.T.);
#15213=ORIENTED_EDGE('',*,*,#11115,.F.);
#15214=ORIENTED_EDGE('',*,*,#11118,.T.);
#15215=ORIENTED_EDGE('',*,*,#11192,.T.);
#15216=ORIENTED_EDGE('',*,*,#11177,.T.);
#15217=ORIENTED_EDGE('',*,*,#11121,.F.);
#15218=ORIENTED_EDGE('',*,*,#11125,.T.);
#15219=ORIENTED_EDGE('',*,*,#11128,.F.);
#15220=ORIENTED_EDGE('',*,*,#11131,.T.);
#15221=ORIENTED_EDGE('',*,*,#11193,.T.);
#15222=ORIENTED_EDGE('',*,*,#11194,.T.);
#15223=ORIENTED_EDGE('',*,*,#11134,.F.);
#15224=ORIENTED_EDGE('',*,*,#11138,.T.);
#15225=ORIENTED_EDGE('',*,*,#11141,.F.);
#15226=ORIENTED_EDGE('',*,*,#11144,.T.);
#15227=ORIENTED_EDGE('',*,*,#11186,.T.);
#15228=ORIENTED_EDGE('',*,*,#11174,.T.);
#15229=ORIENTED_EDGE('',*,*,#11147,.F.);
#15230=ORIENTED_EDGE('',*,*,#11151,.T.);
#15231=ORIENTED_EDGE('',*,*,#11154,.F.);
#15232=ORIENTED_EDGE('',*,*,#11157,.T.);
#15233=ORIENTED_EDGE('',*,*,#11195,.T.);
#15234=ORIENTED_EDGE('',*,*,#11130,.T.);
#15235=ORIENTED_EDGE('',*,*,#11196,.F.);
#15236=ORIENTED_EDGE('',*,*,#11197,.T.);
#15237=ORIENTED_EDGE('',*,*,#11193,.F.);
#15238=ORIENTED_EDGE('',*,*,#11181,.T.);
#15239=ORIENTED_EDGE('',*,*,#11191,.F.);
#15240=ORIENTED_EDGE('',*,*,#11198,.T.);
#15241=ORIENTED_EDGE('',*,*,#11199,.F.);
#15242=ORIENTED_EDGE('',*,*,#11135,.F.);
#15243=ORIENTED_EDGE('',*,*,#11194,.F.);
#15244=ORIENTED_EDGE('',*,*,#11197,.F.);
#15245=ORIENTED_EDGE('',*,*,#11200,.F.);
#15246=ORIENTED_EDGE('',*,*,#11172,.T.);
#15247=ORIENTED_EDGE('',*,*,#11195,.F.);
#15248=ORIENTED_EDGE('',*,*,#11156,.T.);
#15249=ORIENTED_EDGE('',*,*,#11201,.F.);
#15250=ORIENTED_EDGE('',*,*,#11184,.F.);
#15251=ORIENTED_EDGE('',*,*,#11202,.F.);
#15252=ORIENTED_EDGE('',*,*,#11203,.F.);
#15253=ORIENTED_EDGE('',*,*,#11188,.F.);
#15254=ORIENTED_EDGE('',*,*,#11203,.T.);
#15255=ORIENTED_EDGE('',*,*,#11204,.F.);
#15256=ORIENTED_EDGE('',*,*,#11205,.F.);
#15257=ORIENTED_EDGE('',*,*,#11189,.F.);
#15258=ORIENTED_EDGE('',*,*,#11205,.T.);
#15259=ORIENTED_EDGE('',*,*,#11206,.F.);
#15260=ORIENTED_EDGE('',*,*,#11198,.F.);
#15261=ORIENTED_EDGE('',*,*,#11190,.F.);
#15262=ORIENTED_EDGE('',*,*,#11178,.T.);
#15263=ORIENTED_EDGE('',*,*,#11192,.F.);
#15264=ORIENTED_EDGE('',*,*,#11117,.T.);
#15265=ORIENTED_EDGE('',*,*,#11207,.F.);
#15266=ORIENTED_EDGE('',*,*,#11173,.T.);
#15267=ORIENTED_EDGE('',*,*,#11201,.T.);
#15268=ORIENTED_EDGE('',*,*,#11155,.T.);
#15269=ORIENTED_EDGE('',*,*,#11152,.F.);
#15270=ORIENTED_EDGE('',*,*,#11149,.T.);
#15271=ORIENTED_EDGE('',*,*,#11145,.F.);
#15272=ORIENTED_EDGE('',*,*,#11176,.T.);
#15273=ORIENTED_EDGE('',*,*,#11187,.T.);
#15274=ORIENTED_EDGE('',*,*,#11142,.T.);
#15275=ORIENTED_EDGE('',*,*,#11139,.F.);
#15276=ORIENTED_EDGE('',*,*,#11136,.T.);
#15277=ORIENTED_EDGE('',*,*,#11132,.F.);
#15278=ORIENTED_EDGE('',*,*,#11200,.T.);
#15279=ORIENTED_EDGE('',*,*,#11196,.T.);
#15280=ORIENTED_EDGE('',*,*,#11129,.T.);
#15281=ORIENTED_EDGE('',*,*,#11126,.F.);
#15282=ORIENTED_EDGE('',*,*,#11123,.T.);
#15283=ORIENTED_EDGE('',*,*,#11119,.F.);
#15284=ORIENTED_EDGE('',*,*,#11179,.T.);
#15285=ORIENTED_EDGE('',*,*,#11207,.T.);
#15286=ORIENTED_EDGE('',*,*,#11116,.T.);
#15287=ORIENTED_EDGE('',*,*,#11113,.F.);
#15288=ORIENTED_EDGE('',*,*,#11110,.T.);
#15289=ORIENTED_EDGE('',*,*,#11106,.F.);
#15290=ORIENTED_EDGE('',*,*,#11182,.T.);
#15291=ORIENTED_EDGE('',*,*,#11199,.T.);
#15292=ORIENTED_EDGE('',*,*,#11206,.T.);
#15293=ORIENTED_EDGE('',*,*,#11204,.T.);
#15294=ORIENTED_EDGE('',*,*,#11202,.T.);
#15295=ORIENTED_EDGE('',*,*,#11183,.T.);
#15296=ORIENTED_EDGE('',*,*,#11168,.T.);
#15297=ORIENTED_EDGE('',*,*,#11165,.F.);
#15298=ORIENTED_EDGE('',*,*,#11162,.T.);
#15299=ORIENTED_EDGE('',*,*,#11158,.F.);
#15300=ORIENTED_EDGE('',*,*,#11208,.F.);
#15301=ORIENTED_EDGE('',*,*,#11209,.F.);
#15302=ORIENTED_EDGE('',*,*,#11210,.F.);
#15303=ORIENTED_EDGE('',*,*,#11211,.F.);
#15304=ORIENTED_EDGE('',*,*,#11212,.F.);
#15305=ORIENTED_EDGE('',*,*,#11213,.F.);
#15306=ORIENTED_EDGE('',*,*,#11214,.F.);
#15307=ORIENTED_EDGE('',*,*,#11215,.F.);
#15308=ORIENTED_EDGE('',*,*,#11216,.F.);
#15309=ORIENTED_EDGE('',*,*,#11209,.T.);
#15310=ORIENTED_EDGE('',*,*,#11217,.F.);
#15311=ORIENTED_EDGE('',*,*,#11218,.F.);
#15312=ORIENTED_EDGE('',*,*,#11219,.F.);
#15313=ORIENTED_EDGE('',*,*,#11220,.F.);
#15314=ORIENTED_EDGE('',*,*,#11221,.F.);
#15315=ORIENTED_EDGE('',*,*,#11222,.F.);
#15316=ORIENTED_EDGE('',*,*,#11223,.F.);
#15317=ORIENTED_EDGE('',*,*,#11224,.F.);
#15318=ORIENTED_EDGE('',*,*,#11225,.F.);
#15319=ORIENTED_EDGE('',*,*,#11218,.T.);
#15320=ORIENTED_EDGE('',*,*,#11226,.F.);
#15321=ORIENTED_EDGE('',*,*,#11227,.F.);
#15322=ORIENTED_EDGE('',*,*,#11228,.F.);
#15323=ORIENTED_EDGE('',*,*,#11229,.F.);
#15324=ORIENTED_EDGE('',*,*,#11230,.F.);
#15325=ORIENTED_EDGE('',*,*,#11231,.F.);
#15326=ORIENTED_EDGE('',*,*,#11232,.F.);
#15327=ORIENTED_EDGE('',*,*,#11233,.F.);
#15328=ORIENTED_EDGE('',*,*,#11234,.F.);
#15329=ORIENTED_EDGE('',*,*,#11227,.T.);
#15330=ORIENTED_EDGE('',*,*,#11235,.F.);
#15331=ORIENTED_EDGE('',*,*,#11236,.F.);
#15332=ORIENTED_EDGE('',*,*,#11237,.F.);
#15333=ORIENTED_EDGE('',*,*,#11238,.F.);
#15334=ORIENTED_EDGE('',*,*,#11239,.F.);
#15335=ORIENTED_EDGE('',*,*,#11240,.F.);
#15336=ORIENTED_EDGE('',*,*,#11241,.F.);
#15337=ORIENTED_EDGE('',*,*,#11242,.F.);
#15338=ORIENTED_EDGE('',*,*,#11243,.F.);
#15339=ORIENTED_EDGE('',*,*,#11236,.T.);
#15340=ORIENTED_EDGE('',*,*,#11244,.F.);
#15341=ORIENTED_EDGE('',*,*,#11245,.F.);
#15342=ORIENTED_EDGE('',*,*,#11246,.F.);
#15343=ORIENTED_EDGE('',*,*,#11213,.T.);
#15344=ORIENTED_EDGE('',*,*,#11247,.F.);
#15345=ORIENTED_EDGE('',*,*,#11248,.F.);
#15346=ORIENTED_EDGE('',*,*,#11249,.F.);
#15347=ORIENTED_EDGE('',*,*,#11222,.T.);
#15348=ORIENTED_EDGE('',*,*,#11250,.F.);
#15349=ORIENTED_EDGE('',*,*,#11251,.F.);
#15350=ORIENTED_EDGE('',*,*,#11252,.F.);
#15351=ORIENTED_EDGE('',*,*,#11231,.T.);
#15352=ORIENTED_EDGE('',*,*,#11253,.F.);
#15353=ORIENTED_EDGE('',*,*,#11254,.F.);
#15354=ORIENTED_EDGE('',*,*,#11255,.F.);
#15355=ORIENTED_EDGE('',*,*,#11240,.T.);
#15356=ORIENTED_EDGE('',*,*,#11211,.T.);
#15357=ORIENTED_EDGE('',*,*,#11256,.F.);
#15358=ORIENTED_EDGE('',*,*,#11248,.T.);
#15359=ORIENTED_EDGE('',*,*,#11257,.T.);
#15360=ORIENTED_EDGE('',*,*,#11210,.T.);
#15361=ORIENTED_EDGE('',*,*,#11216,.T.);
#15362=ORIENTED_EDGE('',*,*,#11258,.T.);
#15363=ORIENTED_EDGE('',*,*,#11223,.T.);
#15364=ORIENTED_EDGE('',*,*,#11249,.T.);
#15365=ORIENTED_EDGE('',*,*,#11256,.T.);
#15366=ORIENTED_EDGE('',*,*,#11220,.T.);
#15367=ORIENTED_EDGE('',*,*,#11259,.F.);
#15368=ORIENTED_EDGE('',*,*,#11251,.T.);
#15369=ORIENTED_EDGE('',*,*,#11260,.T.);
#15370=ORIENTED_EDGE('',*,*,#11219,.T.);
#15371=ORIENTED_EDGE('',*,*,#11225,.T.);
#15372=ORIENTED_EDGE('',*,*,#11261,.T.);
#15373=ORIENTED_EDGE('',*,*,#11232,.T.);
#15374=ORIENTED_EDGE('',*,*,#11252,.T.);
#15375=ORIENTED_EDGE('',*,*,#11259,.T.);
#15376=ORIENTED_EDGE('',*,*,#11229,.T.);
#15377=ORIENTED_EDGE('',*,*,#11262,.F.);
#15378=ORIENTED_EDGE('',*,*,#11254,.T.);
#15379=ORIENTED_EDGE('',*,*,#11263,.T.);
#15380=ORIENTED_EDGE('',*,*,#11244,.T.);
#15381=ORIENTED_EDGE('',*,*,#11212,.T.);
#15382=ORIENTED_EDGE('',*,*,#11208,.T.);
#15383=ORIENTED_EDGE('',*,*,#11257,.F.);
#15384=ORIENTED_EDGE('',*,*,#11247,.T.);
#15385=ORIENTED_EDGE('',*,*,#11221,.T.);
#15386=ORIENTED_EDGE('',*,*,#11217,.T.);
#15387=ORIENTED_EDGE('',*,*,#11260,.F.);
#15388=ORIENTED_EDGE('',*,*,#11250,.T.);
#15389=ORIENTED_EDGE('',*,*,#11230,.T.);
#15390=ORIENTED_EDGE('',*,*,#11226,.T.);
#15391=ORIENTED_EDGE('',*,*,#11263,.F.);
#15392=ORIENTED_EDGE('',*,*,#11253,.T.);
#15393=ORIENTED_EDGE('',*,*,#11239,.T.);
#15394=ORIENTED_EDGE('',*,*,#11235,.T.);
#15395=ORIENTED_EDGE('',*,*,#11264,.F.);
#15396=ORIENTED_EDGE('',*,*,#11265,.T.);
#15397=ORIENTED_EDGE('',*,*,#11266,.T.);
#15398=ORIENTED_EDGE('',*,*,#11267,.T.);
#15399=ORIENTED_EDGE('',*,*,#11268,.T.);
#15400=ORIENTED_EDGE('',*,*,#11269,.T.);
#15401=ORIENTED_EDGE('',*,*,#11270,.T.);
#15402=ORIENTED_EDGE('',*,*,#11271,.T.);
#15403=ORIENTED_EDGE('',*,*,#11272,.T.);
#15404=ORIENTED_EDGE('',*,*,#11273,.T.);
#15405=ORIENTED_EDGE('',*,*,#11274,.T.);
#15406=ORIENTED_EDGE('',*,*,#11275,.T.);
#15407=ORIENTED_EDGE('',*,*,#11276,.T.);
#15408=ORIENTED_EDGE('',*,*,#11228,.T.);
#15409=ORIENTED_EDGE('',*,*,#11234,.T.);
#15410=ORIENTED_EDGE('',*,*,#11277,.T.);
#15411=ORIENTED_EDGE('',*,*,#11241,.T.);
#15412=ORIENTED_EDGE('',*,*,#11255,.T.);
#15413=ORIENTED_EDGE('',*,*,#11262,.T.);
#15414=ORIENTED_EDGE('',*,*,#11215,.T.);
#15415=ORIENTED_EDGE('',*,*,#11278,.F.);
#15416=ORIENTED_EDGE('',*,*,#11242,.T.);
#15417=ORIENTED_EDGE('',*,*,#11277,.F.);
#15418=ORIENTED_EDGE('',*,*,#11233,.T.);
#15419=ORIENTED_EDGE('',*,*,#11261,.F.);
#15420=ORIENTED_EDGE('',*,*,#11224,.T.);
#15421=ORIENTED_EDGE('',*,*,#11258,.F.);
#15422=ORIENTED_EDGE('',*,*,#11279,.T.);
#15423=ORIENTED_EDGE('',*,*,#11280,.T.);
#15424=ORIENTED_EDGE('',*,*,#11281,.T.);
#15425=ORIENTED_EDGE('',*,*,#11282,.T.);
#15426=ORIENTED_EDGE('',*,*,#11283,.T.);
#15427=ORIENTED_EDGE('',*,*,#11284,.T.);
#15428=ORIENTED_EDGE('',*,*,#11285,.T.);
#15429=ORIENTED_EDGE('',*,*,#11286,.T.);
#15430=ORIENTED_EDGE('',*,*,#11287,.F.);
#15431=ORIENTED_EDGE('',*,*,#11288,.T.);
#15432=ORIENTED_EDGE('',*,*,#11289,.T.);
#15433=ORIENTED_EDGE('',*,*,#11290,.T.);
#15434=ORIENTED_EDGE('',*,*,#11285,.F.);
#15435=ORIENTED_EDGE('',*,*,#11291,.T.);
#15436=ORIENTED_EDGE('',*,*,#11292,.T.);
#15437=ORIENTED_EDGE('',*,*,#11293,.T.);
#15438=ORIENTED_EDGE('',*,*,#11289,.F.);
#15439=ORIENTED_EDGE('',*,*,#11294,.T.);
#15440=ORIENTED_EDGE('',*,*,#11292,.F.);
#15441=ORIENTED_EDGE('',*,*,#11295,.T.);
#15442=ORIENTED_EDGE('',*,*,#11296,.T.);
#15443=ORIENTED_EDGE('',*,*,#11297,.T.);
#15444=ORIENTED_EDGE('',*,*,#11296,.F.);
#15445=ORIENTED_EDGE('',*,*,#11298,.T.);
#15446=ORIENTED_EDGE('',*,*,#11299,.T.);
#15447=ORIENTED_EDGE('',*,*,#11300,.T.);
#15448=ORIENTED_EDGE('',*,*,#11299,.F.);
#15449=ORIENTED_EDGE('',*,*,#11301,.T.);
#15450=ORIENTED_EDGE('',*,*,#11302,.T.);
#15451=ORIENTED_EDGE('',*,*,#11303,.T.);
#15452=ORIENTED_EDGE('',*,*,#11302,.F.);
#15453=ORIENTED_EDGE('',*,*,#11304,.T.);
#15454=ORIENTED_EDGE('',*,*,#11305,.T.);
#15455=ORIENTED_EDGE('',*,*,#11306,.T.);
#15456=ORIENTED_EDGE('',*,*,#11305,.F.);
#15457=ORIENTED_EDGE('',*,*,#11307,.T.);
#15458=ORIENTED_EDGE('',*,*,#11287,.T.);
#15459=ORIENTED_EDGE('',*,*,#11300,.F.);
#15460=ORIENTED_EDGE('',*,*,#11308,.F.);
#15461=ORIENTED_EDGE('',*,*,#11271,.F.);
#15462=ORIENTED_EDGE('',*,*,#11309,.T.);
#15463=ORIENTED_EDGE('',*,*,#11303,.F.);
#15464=ORIENTED_EDGE('',*,*,#11310,.F.);
#15465=ORIENTED_EDGE('',*,*,#11272,.F.);
#15466=ORIENTED_EDGE('',*,*,#11308,.T.);
#15467=ORIENTED_EDGE('',*,*,#11306,.F.);
#15468=ORIENTED_EDGE('',*,*,#11311,.F.);
#15469=ORIENTED_EDGE('',*,*,#11265,.F.);
#15470=ORIENTED_EDGE('',*,*,#11310,.T.);
#15471=ORIENTED_EDGE('',*,*,#11286,.F.);
#15472=ORIENTED_EDGE('',*,*,#11312,.F.);
#15473=ORIENTED_EDGE('',*,*,#11266,.F.);
#15474=ORIENTED_EDGE('',*,*,#11311,.T.);
#15475=ORIENTED_EDGE('',*,*,#11284,.F.);
#15476=ORIENTED_EDGE('',*,*,#11307,.F.);
#15477=ORIENTED_EDGE('',*,*,#11304,.F.);
#15478=ORIENTED_EDGE('',*,*,#11301,.F.);
#15479=ORIENTED_EDGE('',*,*,#11298,.F.);
#15480=ORIENTED_EDGE('',*,*,#11295,.F.);
#15481=ORIENTED_EDGE('',*,*,#11291,.F.);
#15482=ORIENTED_EDGE('',*,*,#11288,.F.);
#15483=ORIENTED_EDGE('',*,*,#11313,.F.);
#15484=ORIENTED_EDGE('',*,*,#11246,.T.);
#15485=ORIENTED_EDGE('',*,*,#11314,.T.);
#15486=ORIENTED_EDGE('',*,*,#11237,.T.);
#15487=ORIENTED_EDGE('',*,*,#11243,.T.);
#15488=ORIENTED_EDGE('',*,*,#11278,.T.);
#15489=ORIENTED_EDGE('',*,*,#11214,.T.);
#15490=ORIENTED_EDGE('',*,*,#11315,.T.);
#15491=ORIENTED_EDGE('',*,*,#11316,.T.);
#15492=ORIENTED_EDGE('',*,*,#11317,.T.);
#15493=ORIENTED_EDGE('',*,*,#11316,.F.);
#15494=ORIENTED_EDGE('',*,*,#11318,.T.);
#15495=ORIENTED_EDGE('',*,*,#11317,.F.);
#15496=ORIENTED_EDGE('',*,*,#11319,.F.);
#15497=ORIENTED_EDGE('',*,*,#11315,.F.);
#15498=ORIENTED_EDGE('',*,*,#11320,.T.);
#15499=ORIENTED_EDGE('',*,*,#11283,.F.);
#15500=ORIENTED_EDGE('',*,*,#11320,.F.);
#15501=ORIENTED_EDGE('',*,*,#11318,.F.);
#15502=ORIENTED_EDGE('',*,*,#11321,.T.);
#15503=ORIENTED_EDGE('',*,*,#11322,.T.);
#15504=ORIENTED_EDGE('',*,*,#11319,.T.);
#15505=ORIENTED_EDGE('',*,*,#11322,.F.);
#15506=ORIENTED_EDGE('',*,*,#11323,.T.);
#15507=ORIENTED_EDGE('',*,*,#11324,.F.);
#15508=ORIENTED_EDGE('',*,*,#11325,.T.);
#15509=ORIENTED_EDGE('',*,*,#11323,.F.);
#15510=ORIENTED_EDGE('',*,*,#11321,.F.);
#15511=ORIENTED_EDGE('',*,*,#11325,.F.);
#15512=ORIENTED_EDGE('',*,*,#11324,.T.);
#15513=ORIENTED_EDGE('',*,*,#11326,.T.);
#15514=ORIENTED_EDGE('',*,*,#11327,.T.);
#15515=ORIENTED_EDGE('',*,*,#11326,.F.);
#15516=ORIENTED_EDGE('',*,*,#11328,.F.);
#15517=ORIENTED_EDGE('',*,*,#11327,.F.);
#15518=ORIENTED_EDGE('',*,*,#11329,.T.);
#15519=ORIENTED_EDGE('',*,*,#11330,.T.);
#15520=ORIENTED_EDGE('',*,*,#11331,.T.);
#15521=ORIENTED_EDGE('',*,*,#11330,.F.);
#15522=ORIENTED_EDGE('',*,*,#11331,.F.);
#15523=ORIENTED_EDGE('',*,*,#11332,.F.);
#15524=ORIENTED_EDGE('',*,*,#11313,.T.);
#15525=ORIENTED_EDGE('',*,*,#11333,.T.);
#15526=ORIENTED_EDGE('',*,*,#11329,.F.);
#15527=ORIENTED_EDGE('',*,*,#11333,.F.);
#15528=ORIENTED_EDGE('',*,*,#11334,.T.);
#15529=ORIENTED_EDGE('',*,*,#11335,.T.);
#15530=ORIENTED_EDGE('',*,*,#11332,.T.);
#15531=ORIENTED_EDGE('',*,*,#11335,.F.);
#15532=ORIENTED_EDGE('',*,*,#11336,.T.);
#15533=ORIENTED_EDGE('',*,*,#11334,.F.);
#15534=ORIENTED_EDGE('',*,*,#11337,.T.);
#15535=ORIENTED_EDGE('',*,*,#11338,.T.);
#15536=ORIENTED_EDGE('',*,*,#11337,.F.);
#15537=ORIENTED_EDGE('',*,*,#11336,.F.);
#15538=ORIENTED_EDGE('',*,*,#11276,.F.);
#15539=ORIENTED_EDGE('',*,*,#11339,.T.);
#15540=ORIENTED_EDGE('',*,*,#11279,.F.);
#15541=ORIENTED_EDGE('',*,*,#11339,.F.);
#15542=ORIENTED_EDGE('',*,*,#11275,.F.);
#15543=ORIENTED_EDGE('',*,*,#11340,.T.);
#15544=ORIENTED_EDGE('',*,*,#11280,.F.);
#15545=ORIENTED_EDGE('',*,*,#11340,.F.);
#15546=ORIENTED_EDGE('',*,*,#11274,.F.);
#15547=ORIENTED_EDGE('',*,*,#11341,.T.);
#15548=ORIENTED_EDGE('',*,*,#11281,.F.);
#15549=ORIENTED_EDGE('',*,*,#11341,.F.);
#15550=ORIENTED_EDGE('',*,*,#11273,.F.);
#15551=ORIENTED_EDGE('',*,*,#11342,.T.);
#15552=ORIENTED_EDGE('',*,*,#11282,.F.);
#15553=ORIENTED_EDGE('',*,*,#11342,.F.);
#15554=ORIENTED_EDGE('',*,*,#11343,.F.);
#15555=ORIENTED_EDGE('',*,*,#11344,.T.);
#15556=ORIENTED_EDGE('',*,*,#11328,.T.);
#15557=ORIENTED_EDGE('',*,*,#11344,.F.);
#15558=ORIENTED_EDGE('',*,*,#11338,.F.);
#15559=ORIENTED_EDGE('',*,*,#11343,.T.);
#15560=ORIENTED_EDGE('',*,*,#11297,.F.);
#15561=ORIENTED_EDGE('',*,*,#11309,.F.);
#15562=ORIENTED_EDGE('',*,*,#11270,.F.);
#15563=ORIENTED_EDGE('',*,*,#11345,.T.);
#15564=ORIENTED_EDGE('',*,*,#11294,.F.);
#15565=ORIENTED_EDGE('',*,*,#11345,.F.);
#15566=ORIENTED_EDGE('',*,*,#11269,.F.);
#15567=ORIENTED_EDGE('',*,*,#11346,.T.);
#15568=ORIENTED_EDGE('',*,*,#11293,.F.);
#15569=ORIENTED_EDGE('',*,*,#11346,.F.);
#15570=ORIENTED_EDGE('',*,*,#11268,.F.);
#15571=ORIENTED_EDGE('',*,*,#11347,.T.);
#15572=ORIENTED_EDGE('',*,*,#11290,.F.);
#15573=ORIENTED_EDGE('',*,*,#11347,.F.);
#15574=ORIENTED_EDGE('',*,*,#11267,.F.);
#15575=ORIENTED_EDGE('',*,*,#11312,.T.);
#15576=ORIENTED_EDGE('',*,*,#11245,.T.);
#15577=ORIENTED_EDGE('',*,*,#11264,.T.);
#15578=ORIENTED_EDGE('',*,*,#11238,.T.);
#15579=ORIENTED_EDGE('',*,*,#11314,.F.);
#15580=ORIENTED_EDGE('',*,*,#11348,.T.);
#15581=ORIENTED_EDGE('',*,*,#11349,.T.);
#15582=ORIENTED_EDGE('',*,*,#11350,.T.);
#15583=ORIENTED_EDGE('',*,*,#11351,.T.);
#15584=ORIENTED_EDGE('',*,*,#11349,.F.);
#15585=ORIENTED_EDGE('',*,*,#11352,.F.);
#15586=ORIENTED_EDGE('',*,*,#11353,.F.);
#15587=ORIENTED_EDGE('',*,*,#11354,.F.);
#15588=ORIENTED_EDGE('',*,*,#11355,.T.);
#15589=ORIENTED_EDGE('',*,*,#11356,.T.);
#15590=ORIENTED_EDGE('',*,*,#11357,.T.);
#15591=ORIENTED_EDGE('',*,*,#11353,.T.);
#15592=ORIENTED_EDGE('',*,*,#11356,.F.);
#15593=ORIENTED_EDGE('',*,*,#11358,.F.);
#15594=ORIENTED_EDGE('',*,*,#11359,.F.);
#15595=ORIENTED_EDGE('',*,*,#11360,.F.);
#15596=ORIENTED_EDGE('',*,*,#11361,.T.);
#15597=ORIENTED_EDGE('',*,*,#11362,.T.);
#15598=ORIENTED_EDGE('',*,*,#11363,.T.);
#15599=ORIENTED_EDGE('',*,*,#11364,.T.);
#15600=ORIENTED_EDGE('',*,*,#11362,.F.);
#15601=ORIENTED_EDGE('',*,*,#11365,.F.);
#15602=ORIENTED_EDGE('',*,*,#11366,.F.);
#15603=ORIENTED_EDGE('',*,*,#11367,.F.);
#15604=ORIENTED_EDGE('',*,*,#11368,.T.);
#15605=ORIENTED_EDGE('',*,*,#11369,.T.);
#15606=ORIENTED_EDGE('',*,*,#11370,.T.);
#15607=ORIENTED_EDGE('',*,*,#11366,.T.);
#15608=ORIENTED_EDGE('',*,*,#11369,.F.);
#15609=ORIENTED_EDGE('',*,*,#11371,.F.);
#15610=ORIENTED_EDGE('',*,*,#11372,.F.);
#15611=ORIENTED_EDGE('',*,*,#11373,.F.);
#15612=ORIENTED_EDGE('',*,*,#11374,.T.);
#15613=ORIENTED_EDGE('',*,*,#11375,.T.);
#15614=ORIENTED_EDGE('',*,*,#11376,.T.);
#15615=ORIENTED_EDGE('',*,*,#11377,.T.);
#15616=ORIENTED_EDGE('',*,*,#11375,.F.);
#15617=ORIENTED_EDGE('',*,*,#11378,.F.);
#15618=ORIENTED_EDGE('',*,*,#11379,.F.);
#15619=ORIENTED_EDGE('',*,*,#11380,.F.);
#15620=ORIENTED_EDGE('',*,*,#11381,.T.);
#15621=ORIENTED_EDGE('',*,*,#11382,.T.);
#15622=ORIENTED_EDGE('',*,*,#11383,.T.);
#15623=ORIENTED_EDGE('',*,*,#11379,.T.);
#15624=ORIENTED_EDGE('',*,*,#11382,.F.);
#15625=ORIENTED_EDGE('',*,*,#11384,.F.);
#15626=ORIENTED_EDGE('',*,*,#11385,.F.);
#15627=ORIENTED_EDGE('',*,*,#11386,.F.);
#15628=ORIENTED_EDGE('',*,*,#11387,.T.);
#15629=ORIENTED_EDGE('',*,*,#11388,.T.);
#15630=ORIENTED_EDGE('',*,*,#11389,.T.);
#15631=ORIENTED_EDGE('',*,*,#11390,.T.);
#15632=ORIENTED_EDGE('',*,*,#11388,.F.);
#15633=ORIENTED_EDGE('',*,*,#11391,.F.);
#15634=ORIENTED_EDGE('',*,*,#11392,.F.);
#15635=ORIENTED_EDGE('',*,*,#11393,.F.);
#15636=ORIENTED_EDGE('',*,*,#11394,.T.);
#15637=ORIENTED_EDGE('',*,*,#11395,.T.);
#15638=ORIENTED_EDGE('',*,*,#11396,.T.);
#15639=ORIENTED_EDGE('',*,*,#11392,.T.);
#15640=ORIENTED_EDGE('',*,*,#11395,.F.);
#15641=ORIENTED_EDGE('',*,*,#11397,.F.);
#15642=ORIENTED_EDGE('',*,*,#11398,.F.);
#15643=ORIENTED_EDGE('',*,*,#11399,.F.);
#15644=ORIENTED_EDGE('',*,*,#11400,.T.);
#15645=ORIENTED_EDGE('',*,*,#11401,.T.);
#15646=ORIENTED_EDGE('',*,*,#11402,.T.);
#15647=ORIENTED_EDGE('',*,*,#11403,.T.);
#15648=ORIENTED_EDGE('',*,*,#11401,.F.);
#15649=ORIENTED_EDGE('',*,*,#11404,.F.);
#15650=ORIENTED_EDGE('',*,*,#11405,.F.);
#15651=ORIENTED_EDGE('',*,*,#11406,.F.);
#15652=ORIENTED_EDGE('',*,*,#11407,.T.);
#15653=ORIENTED_EDGE('',*,*,#11408,.T.);
#15654=ORIENTED_EDGE('',*,*,#11409,.T.);
#15655=ORIENTED_EDGE('',*,*,#11405,.T.);
#15656=ORIENTED_EDGE('',*,*,#11408,.F.);
#15657=ORIENTED_EDGE('',*,*,#11410,.F.);
#15658=ORIENTED_EDGE('',*,*,#11411,.F.);
#15659=ORIENTED_EDGE('',*,*,#11412,.F.);
#15660=ORIENTED_EDGE('',*,*,#11403,.F.);
#15661=ORIENTED_EDGE('',*,*,#11413,.F.);
#15662=ORIENTED_EDGE('',*,*,#11414,.F.);
#15663=ORIENTED_EDGE('',*,*,#11415,.F.);
#15664=ORIENTED_EDGE('',*,*,#11390,.F.);
#15665=ORIENTED_EDGE('',*,*,#11416,.F.);
#15666=ORIENTED_EDGE('',*,*,#11417,.F.);
#15667=ORIENTED_EDGE('',*,*,#11418,.F.);
#15668=ORIENTED_EDGE('',*,*,#11364,.F.);
#15669=ORIENTED_EDGE('',*,*,#11419,.F.);
#15670=ORIENTED_EDGE('',*,*,#11420,.F.);
#15671=ORIENTED_EDGE('',*,*,#11421,.F.);
#15672=ORIENTED_EDGE('',*,*,#11351,.F.);
#15673=ORIENTED_EDGE('',*,*,#11422,.F.);
#15674=ORIENTED_EDGE('',*,*,#11423,.F.);
#15675=ORIENTED_EDGE('',*,*,#11424,.F.);
#15676=ORIENTED_EDGE('',*,*,#11411,.T.);
#15677=ORIENTED_EDGE('',*,*,#11425,.F.);
#15678=ORIENTED_EDGE('',*,*,#11426,.T.);
#15679=ORIENTED_EDGE('',*,*,#11427,.F.);
#15680=ORIENTED_EDGE('',*,*,#11417,.T.);
#15681=ORIENTED_EDGE('',*,*,#11428,.F.);
#15682=ORIENTED_EDGE('',*,*,#11385,.T.);
#15683=ORIENTED_EDGE('',*,*,#11429,.F.);
#15684=ORIENTED_EDGE('',*,*,#11413,.T.);
#15685=ORIENTED_EDGE('',*,*,#11402,.F.);
#15686=ORIENTED_EDGE('',*,*,#11406,.T.);
#15687=ORIENTED_EDGE('',*,*,#11409,.F.);
#15688=ORIENTED_EDGE('',*,*,#11412,.T.);
#15689=ORIENTED_EDGE('',*,*,#11427,.T.);
#15690=ORIENTED_EDGE('',*,*,#11430,.T.);
#15691=ORIENTED_EDGE('',*,*,#11431,.T.);
#15692=ORIENTED_EDGE('',*,*,#11432,.T.);
#15693=ORIENTED_EDGE('',*,*,#11433,.T.);
#15694=ORIENTED_EDGE('',*,*,#11422,.T.);
#15695=ORIENTED_EDGE('',*,*,#11350,.F.);
#15696=ORIENTED_EDGE('',*,*,#11354,.T.);
#15697=ORIENTED_EDGE('',*,*,#11357,.F.);
#15698=ORIENTED_EDGE('',*,*,#11360,.T.);
#15699=ORIENTED_EDGE('',*,*,#11434,.T.);
#15700=ORIENTED_EDGE('',*,*,#11419,.T.);
#15701=ORIENTED_EDGE('',*,*,#11363,.F.);
#15702=ORIENTED_EDGE('',*,*,#11367,.T.);
#15703=ORIENTED_EDGE('',*,*,#11370,.F.);
#15704=ORIENTED_EDGE('',*,*,#11373,.T.);
#15705=ORIENTED_EDGE('',*,*,#11435,.T.);
#15706=ORIENTED_EDGE('',*,*,#11436,.T.);
#15707=ORIENTED_EDGE('',*,*,#11376,.F.);
#15708=ORIENTED_EDGE('',*,*,#11380,.T.);
#15709=ORIENTED_EDGE('',*,*,#11383,.F.);
#15710=ORIENTED_EDGE('',*,*,#11386,.T.);
#15711=ORIENTED_EDGE('',*,*,#11428,.T.);
#15712=ORIENTED_EDGE('',*,*,#11416,.T.);
#15713=ORIENTED_EDGE('',*,*,#11389,.F.);
#15714=ORIENTED_EDGE('',*,*,#11393,.T.);
#15715=ORIENTED_EDGE('',*,*,#11396,.F.);
#15716=ORIENTED_EDGE('',*,*,#11399,.T.);
#15717=ORIENTED_EDGE('',*,*,#11437,.T.);
#15718=ORIENTED_EDGE('',*,*,#11372,.T.);
#15719=ORIENTED_EDGE('',*,*,#11438,.F.);
#15720=ORIENTED_EDGE('',*,*,#11439,.T.);
#15721=ORIENTED_EDGE('',*,*,#11435,.F.);
#15722=ORIENTED_EDGE('',*,*,#11423,.T.);
#15723=ORIENTED_EDGE('',*,*,#11433,.F.);
#15724=ORIENTED_EDGE('',*,*,#11440,.T.);
#15725=ORIENTED_EDGE('',*,*,#11441,.F.);
#15726=ORIENTED_EDGE('',*,*,#11377,.F.);
#15727=ORIENTED_EDGE('',*,*,#11436,.F.);
#15728=ORIENTED_EDGE('',*,*,#11439,.F.);
#15729=ORIENTED_EDGE('',*,*,#11442,.F.);
#15730=ORIENTED_EDGE('',*,*,#11414,.T.);
#15731=ORIENTED_EDGE('',*,*,#11437,.F.);
#15732=ORIENTED_EDGE('',*,*,#11398,.T.);
#15733=ORIENTED_EDGE('',*,*,#11443,.F.);
#15734=ORIENTED_EDGE('',*,*,#11426,.F.);
#15735=ORIENTED_EDGE('',*,*,#11444,.F.);
#15736=ORIENTED_EDGE('',*,*,#11445,.F.);
#15737=ORIENTED_EDGE('',*,*,#11430,.F.);
#15738=ORIENTED_EDGE('',*,*,#11445,.T.);
#15739=ORIENTED_EDGE('',*,*,#11446,.F.);
#15740=ORIENTED_EDGE('',*,*,#11447,.F.);
#15741=ORIENTED_EDGE('',*,*,#11431,.F.);
#15742=ORIENTED_EDGE('',*,*,#11447,.T.);
#15743=ORIENTED_EDGE('',*,*,#11448,.F.);
#15744=ORIENTED_EDGE('',*,*,#11440,.F.);
#15745=ORIENTED_EDGE('',*,*,#11432,.F.);
#15746=ORIENTED_EDGE('',*,*,#11420,.T.);
#15747=ORIENTED_EDGE('',*,*,#11434,.F.);
#15748=ORIENTED_EDGE('',*,*,#11359,.T.);
#15749=ORIENTED_EDGE('',*,*,#11449,.F.);
#15750=ORIENTED_EDGE('',*,*,#11415,.T.);
#15751=ORIENTED_EDGE('',*,*,#11443,.T.);
#15752=ORIENTED_EDGE('',*,*,#11397,.T.);
#15753=ORIENTED_EDGE('',*,*,#11394,.F.);
#15754=ORIENTED_EDGE('',*,*,#11391,.T.);
#15755=ORIENTED_EDGE('',*,*,#11387,.F.);
#15756=ORIENTED_EDGE('',*,*,#11418,.T.);
#15757=ORIENTED_EDGE('',*,*,#11429,.T.);
#15758=ORIENTED_EDGE('',*,*,#11384,.T.);
#15759=ORIENTED_EDGE('',*,*,#11381,.F.);
#15760=ORIENTED_EDGE('',*,*,#11378,.T.);
#15761=ORIENTED_EDGE('',*,*,#11374,.F.);
#15762=ORIENTED_EDGE('',*,*,#11442,.T.);
#15763=ORIENTED_EDGE('',*,*,#11438,.T.);
#15764=ORIENTED_EDGE('',*,*,#11371,.T.);
#15765=ORIENTED_EDGE('',*,*,#11368,.F.);
#15766=ORIENTED_EDGE('',*,*,#11365,.T.);
#15767=ORIENTED_EDGE('',*,*,#11361,.F.);
#15768=ORIENTED_EDGE('',*,*,#11421,.T.);
#15769=ORIENTED_EDGE('',*,*,#11449,.T.);
#15770=ORIENTED_EDGE('',*,*,#11358,.T.);
#15771=ORIENTED_EDGE('',*,*,#11355,.F.);
#15772=ORIENTED_EDGE('',*,*,#11352,.T.);
#15773=ORIENTED_EDGE('',*,*,#11348,.F.);
#15774=ORIENTED_EDGE('',*,*,#11424,.T.);
#15775=ORIENTED_EDGE('',*,*,#11441,.T.);
#15776=ORIENTED_EDGE('',*,*,#11448,.T.);
#15777=ORIENTED_EDGE('',*,*,#11446,.T.);
#15778=ORIENTED_EDGE('',*,*,#11444,.T.);
#15779=ORIENTED_EDGE('',*,*,#11425,.T.);
#15780=ORIENTED_EDGE('',*,*,#11410,.T.);
#15781=ORIENTED_EDGE('',*,*,#11407,.F.);
#15782=ORIENTED_EDGE('',*,*,#11404,.T.);
#15783=ORIENTED_EDGE('',*,*,#11400,.F.);
#15784=ORIENTED_EDGE('',*,*,#11450,.F.);
#15785=ORIENTED_EDGE('',*,*,#11451,.T.);
#15786=ORIENTED_EDGE('',*,*,#11452,.T.);
#15787=ORIENTED_EDGE('',*,*,#11453,.T.);
#15788=ORIENTED_EDGE('',*,*,#11454,.T.);
#15789=ORIENTED_EDGE('',*,*,#11450,.T.);
#15790=ORIENTED_EDGE('',*,*,#11455,.T.);
#15791=ORIENTED_EDGE('',*,*,#11456,.T.);
#15792=ORIENTED_EDGE('',*,*,#11457,.T.);
#15793=ORIENTED_EDGE('',*,*,#11458,.T.);
#15794=ORIENTED_EDGE('',*,*,#11459,.T.);
#15795=ORIENTED_EDGE('',*,*,#11460,.T.);
#15796=ORIENTED_EDGE('',*,*,#11459,.F.);
#15797=ORIENTED_EDGE('',*,*,#11461,.F.);
#15798=ORIENTED_EDGE('',*,*,#11460,.F.);
#15799=ORIENTED_EDGE('',*,*,#11462,.F.);
#15800=ORIENTED_EDGE('',*,*,#11458,.F.);
#15801=ORIENTED_EDGE('',*,*,#11463,.T.);
#15802=ORIENTED_EDGE('',*,*,#11452,.F.);
#15803=ORIENTED_EDGE('',*,*,#11464,.T.);
#15804=ORIENTED_EDGE('',*,*,#11462,.T.);
#15805=ORIENTED_EDGE('',*,*,#11464,.F.);
#15806=ORIENTED_EDGE('',*,*,#11451,.F.);
#15807=ORIENTED_EDGE('',*,*,#11457,.F.);
#15808=ORIENTED_EDGE('',*,*,#11465,.T.);
#15809=ORIENTED_EDGE('',*,*,#11466,.T.);
#15810=ORIENTED_EDGE('',*,*,#11453,.F.);
#15811=ORIENTED_EDGE('',*,*,#11463,.F.);
#15812=ORIENTED_EDGE('',*,*,#11467,.T.);
#15813=ORIENTED_EDGE('',*,*,#11465,.F.);
#15814=ORIENTED_EDGE('',*,*,#11456,.F.);
#15815=ORIENTED_EDGE('',*,*,#11466,.F.);
#15816=ORIENTED_EDGE('',*,*,#11467,.F.);
#15817=ORIENTED_EDGE('',*,*,#11461,.T.);
#15818=ORIENTED_EDGE('',*,*,#11468,.T.);
#15819=ORIENTED_EDGE('',*,*,#11469,.F.);
#15820=ORIENTED_EDGE('',*,*,#11470,.F.);
#15821=ORIENTED_EDGE('',*,*,#11468,.F.);
#15822=ORIENTED_EDGE('',*,*,#11470,.T.);
#15823=ORIENTED_EDGE('',*,*,#11471,.T.);
#15824=ORIENTED_EDGE('',*,*,#11472,.T.);
#15825=ORIENTED_EDGE('',*,*,#11471,.F.);
#15826=ORIENTED_EDGE('',*,*,#11469,.T.);
#15827=ORIENTED_EDGE('',*,*,#11472,.F.);
#15828=ORIENTED_EDGE('',*,*,#11454,.F.);
#15829=ORIENTED_EDGE('',*,*,#11455,.F.);
#15830=ORIENTED_EDGE('',*,*,#11473,.F.);
#15831=ORIENTED_EDGE('',*,*,#11474,.T.);
#15832=ORIENTED_EDGE('',*,*,#11475,.F.);
#15833=ORIENTED_EDGE('',*,*,#11476,.F.);
#15834=ORIENTED_EDGE('',*,*,#11477,.F.);
#15835=ORIENTED_EDGE('',*,*,#11478,.T.);
#15836=ORIENTED_EDGE('',*,*,#11479,.F.);
#15837=ORIENTED_EDGE('',*,*,#11480,.F.);
#15838=ORIENTED_EDGE('',*,*,#11481,.F.);
#15839=ORIENTED_EDGE('',*,*,#11482,.F.);
#15840=ORIENTED_EDGE('',*,*,#11483,.F.);
#15841=ORIENTED_EDGE('',*,*,#11474,.F.);
#15842=ORIENTED_EDGE('',*,*,#11484,.F.);
#15843=ORIENTED_EDGE('',*,*,#11485,.F.);
#15844=ORIENTED_EDGE('',*,*,#11486,.F.);
#15845=ORIENTED_EDGE('',*,*,#11478,.F.);
#15846=ORIENTED_EDGE('',*,*,#11476,.T.);
#15847=ORIENTED_EDGE('',*,*,#11487,.T.);
#15848=ORIENTED_EDGE('',*,*,#11488,.T.);
#15849=ORIENTED_EDGE('',*,*,#11489,.F.);
#15850=ORIENTED_EDGE('',*,*,#11475,.T.);
#15851=ORIENTED_EDGE('',*,*,#11483,.T.);
#15852=ORIENTED_EDGE('',*,*,#11490,.T.);
#15853=ORIENTED_EDGE('',*,*,#11484,.T.);
#15854=ORIENTED_EDGE('',*,*,#11477,.T.);
#15855=ORIENTED_EDGE('',*,*,#11491,.T.);
#15856=ORIENTED_EDGE('',*,*,#11492,.T.);
#15857=ORIENTED_EDGE('',*,*,#11493,.T.);
#15858=ORIENTED_EDGE('',*,*,#11494,.T.);
#15859=ORIENTED_EDGE('',*,*,#11495,.F.);
#15860=ORIENTED_EDGE('',*,*,#11496,.F.);
#15861=ORIENTED_EDGE('',*,*,#11497,.F.);
#15862=ORIENTED_EDGE('',*,*,#11498,.F.);
#15863=ORIENTED_EDGE('',*,*,#11487,.F.);
#15864=ORIENTED_EDGE('',*,*,#11480,.T.);
#15865=ORIENTED_EDGE('',*,*,#11499,.T.);
#15866=ORIENTED_EDGE('',*,*,#11500,.F.);
#15867=ORIENTED_EDGE('',*,*,#11491,.F.);
#15868=ORIENTED_EDGE('',*,*,#11494,.F.);
#15869=ORIENTED_EDGE('',*,*,#11501,.T.);
#15870=ORIENTED_EDGE('',*,*,#11502,.T.);
#15871=ORIENTED_EDGE('',*,*,#11503,.F.);
#15872=ORIENTED_EDGE('',*,*,#11493,.F.);
#15873=ORIENTED_EDGE('',*,*,#11504,.T.);
#15874=ORIENTED_EDGE('',*,*,#11505,.T.);
#15875=ORIENTED_EDGE('',*,*,#11501,.F.);
#15876=ORIENTED_EDGE('',*,*,#11492,.F.);
#15877=ORIENTED_EDGE('',*,*,#11500,.T.);
#15878=ORIENTED_EDGE('',*,*,#11506,.T.);
#15879=ORIENTED_EDGE('',*,*,#11504,.F.);
#15880=ORIENTED_EDGE('',*,*,#11482,.T.);
#15881=ORIENTED_EDGE('',*,*,#11507,.T.);
#15882=ORIENTED_EDGE('',*,*,#11485,.T.);
#15883=ORIENTED_EDGE('',*,*,#11490,.F.);
#15884=ORIENTED_EDGE('',*,*,#11495,.T.);
#15885=ORIENTED_EDGE('',*,*,#11503,.T.);
#15886=ORIENTED_EDGE('',*,*,#11508,.F.);
#15887=ORIENTED_EDGE('',*,*,#11509,.F.);
#15888=ORIENTED_EDGE('',*,*,#11496,.T.);
#15889=ORIENTED_EDGE('',*,*,#11509,.T.);
#15890=ORIENTED_EDGE('',*,*,#11510,.F.);
#15891=ORIENTED_EDGE('',*,*,#11511,.F.);
#15892=ORIENTED_EDGE('',*,*,#11497,.T.);
#15893=ORIENTED_EDGE('',*,*,#11511,.T.);
#15894=ORIENTED_EDGE('',*,*,#11512,.F.);
#15895=ORIENTED_EDGE('',*,*,#11513,.F.);
#15896=ORIENTED_EDGE('',*,*,#11498,.T.);
#15897=ORIENTED_EDGE('',*,*,#11513,.T.);
#15898=ORIENTED_EDGE('',*,*,#11514,.F.);
#15899=ORIENTED_EDGE('',*,*,#11488,.F.);
#15900=ORIENTED_EDGE('',*,*,#11473,.T.);
#15901=ORIENTED_EDGE('',*,*,#11489,.T.);
#15902=ORIENTED_EDGE('',*,*,#11514,.T.);
#15903=ORIENTED_EDGE('',*,*,#11512,.T.);
#15904=ORIENTED_EDGE('',*,*,#11510,.T.);
#15905=ORIENTED_EDGE('',*,*,#11508,.T.);
#15906=ORIENTED_EDGE('',*,*,#11502,.F.);
#15907=ORIENTED_EDGE('',*,*,#11505,.F.);
#15908=ORIENTED_EDGE('',*,*,#11506,.F.);
#15909=ORIENTED_EDGE('',*,*,#11499,.F.);
#15910=ORIENTED_EDGE('',*,*,#11479,.T.);
#15911=ORIENTED_EDGE('',*,*,#11486,.T.);
#15912=ORIENTED_EDGE('',*,*,#11507,.F.);
#15913=ORIENTED_EDGE('',*,*,#11481,.T.);
#15914=ORIENTED_EDGE('',*,*,#11515,.F.);
#15915=ORIENTED_EDGE('',*,*,#11516,.T.);
#15916=ORIENTED_EDGE('',*,*,#11517,.F.);
#15917=ORIENTED_EDGE('',*,*,#11516,.F.);
#15918=ORIENTED_EDGE('',*,*,#11518,.F.);
#15919=ORIENTED_EDGE('',*,*,#11519,.T.);
#15920=ORIENTED_EDGE('',*,*,#11520,.F.);
#15921=ORIENTED_EDGE('',*,*,#11519,.F.);
#15922=ORIENTED_EDGE('',*,*,#11521,.F.);
#15923=ORIENTED_EDGE('',*,*,#11522,.T.);
#15924=ORIENTED_EDGE('',*,*,#11523,.F.);
#15925=ORIENTED_EDGE('',*,*,#11522,.F.);
#15926=ORIENTED_EDGE('',*,*,#11524,.F.);
#15927=ORIENTED_EDGE('',*,*,#11525,.T.);
#15928=ORIENTED_EDGE('',*,*,#11526,.F.);
#15929=ORIENTED_EDGE('',*,*,#11525,.F.);
#15930=ORIENTED_EDGE('',*,*,#11527,.F.);
#15931=ORIENTED_EDGE('',*,*,#11528,.T.);
#15932=ORIENTED_EDGE('',*,*,#11529,.F.);
#15933=ORIENTED_EDGE('',*,*,#11528,.F.);
#15934=ORIENTED_EDGE('',*,*,#11530,.F.);
#15935=ORIENTED_EDGE('',*,*,#11531,.T.);
#15936=ORIENTED_EDGE('',*,*,#11532,.F.);
#15937=ORIENTED_EDGE('',*,*,#11531,.F.);
#15938=ORIENTED_EDGE('',*,*,#11533,.F.);
#15939=ORIENTED_EDGE('',*,*,#11534,.T.);
#15940=ORIENTED_EDGE('',*,*,#11535,.F.);
#15941=ORIENTED_EDGE('',*,*,#11534,.F.);
#15942=ORIENTED_EDGE('',*,*,#11536,.F.);
#15943=ORIENTED_EDGE('',*,*,#11537,.T.);
#15944=ORIENTED_EDGE('',*,*,#11538,.F.);
#15945=ORIENTED_EDGE('',*,*,#11537,.F.);
#15946=ORIENTED_EDGE('',*,*,#11539,.F.);
#15947=ORIENTED_EDGE('',*,*,#11540,.T.);
#15948=ORIENTED_EDGE('',*,*,#11541,.F.);
#15949=ORIENTED_EDGE('',*,*,#11540,.F.);
#15950=ORIENTED_EDGE('',*,*,#11542,.F.);
#15951=ORIENTED_EDGE('',*,*,#11543,.T.);
#15952=ORIENTED_EDGE('',*,*,#11544,.F.);
#15953=ORIENTED_EDGE('',*,*,#11543,.F.);
#15954=ORIENTED_EDGE('',*,*,#11545,.F.);
#15955=ORIENTED_EDGE('',*,*,#11546,.T.);
#15956=ORIENTED_EDGE('',*,*,#11547,.T.);
#15957=ORIENTED_EDGE('',*,*,#11548,.F.);
#15958=ORIENTED_EDGE('',*,*,#11549,.F.);
#15959=ORIENTED_EDGE('',*,*,#11550,.T.);
#15960=ORIENTED_EDGE('',*,*,#11551,.T.);
#15961=ORIENTED_EDGE('',*,*,#11546,.F.);
#15962=ORIENTED_EDGE('',*,*,#11552,.F.);
#15963=ORIENTED_EDGE('',*,*,#11553,.T.);
#15964=ORIENTED_EDGE('',*,*,#11554,.T.);
#15965=ORIENTED_EDGE('',*,*,#11555,.F.);
#15966=ORIENTED_EDGE('',*,*,#11556,.F.);
#15967=ORIENTED_EDGE('',*,*,#11548,.T.);
#15968=ORIENTED_EDGE('',*,*,#11557,.T.);
#15969=ORIENTED_EDGE('',*,*,#11553,.F.);
#15970=ORIENTED_EDGE('',*,*,#11558,.T.);
#15971=ORIENTED_EDGE('',*,*,#11559,.T.);
#15972=ORIENTED_EDGE('',*,*,#11560,.F.);
#15973=ORIENTED_EDGE('',*,*,#11561,.F.);
#15974=ORIENTED_EDGE('',*,*,#11562,.T.);
#15975=ORIENTED_EDGE('',*,*,#11561,.T.);
#15976=ORIENTED_EDGE('',*,*,#11563,.F.);
#15977=ORIENTED_EDGE('',*,*,#11564,.F.);
#15978=ORIENTED_EDGE('',*,*,#11565,.F.);
#15979=ORIENTED_EDGE('',*,*,#11564,.T.);
#15980=ORIENTED_EDGE('',*,*,#11566,.T.);
#15981=ORIENTED_EDGE('',*,*,#11550,.F.);
#15982=ORIENTED_EDGE('',*,*,#11567,.T.);
#15983=ORIENTED_EDGE('',*,*,#11555,.T.);
#15984=ORIENTED_EDGE('',*,*,#11568,.F.);
#15985=ORIENTED_EDGE('',*,*,#11569,.F.);
#15986=ORIENTED_EDGE('',*,*,#11570,.T.);
#15987=ORIENTED_EDGE('',*,*,#11569,.T.);
#15988=ORIENTED_EDGE('',*,*,#11571,.F.);
#15989=ORIENTED_EDGE('',*,*,#11572,.F.);
#15990=ORIENTED_EDGE('',*,*,#11573,.T.);
#15991=ORIENTED_EDGE('',*,*,#11572,.T.);
#15992=ORIENTED_EDGE('',*,*,#11574,.F.);
#15993=ORIENTED_EDGE('',*,*,#11559,.F.);
#15994=ORIENTED_EDGE('',*,*,#11574,.T.);
#15995=ORIENTED_EDGE('',*,*,#11571,.T.);
#15996=ORIENTED_EDGE('',*,*,#11568,.T.);
#15997=ORIENTED_EDGE('',*,*,#11554,.F.);
#15998=ORIENTED_EDGE('',*,*,#11557,.F.);
#15999=ORIENTED_EDGE('',*,*,#11547,.F.);
#16000=ORIENTED_EDGE('',*,*,#11551,.F.);
#16001=ORIENTED_EDGE('',*,*,#11566,.F.);
#16002=ORIENTED_EDGE('',*,*,#11563,.T.);
#16003=ORIENTED_EDGE('',*,*,#11560,.T.);
#16004=ORIENTED_EDGE('',*,*,#11517,.T.);
#16005=ORIENTED_EDGE('',*,*,#11520,.T.);
#16006=ORIENTED_EDGE('',*,*,#11523,.T.);
#16007=ORIENTED_EDGE('',*,*,#11526,.T.);
#16008=ORIENTED_EDGE('',*,*,#11529,.T.);
#16009=ORIENTED_EDGE('',*,*,#11532,.T.);
#16010=ORIENTED_EDGE('',*,*,#11535,.T.);
#16011=ORIENTED_EDGE('',*,*,#11538,.T.);
#16012=ORIENTED_EDGE('',*,*,#11541,.T.);
#16013=ORIENTED_EDGE('',*,*,#11544,.T.);
#16014=ORIENTED_EDGE('',*,*,#11573,.F.);
#16015=ORIENTED_EDGE('',*,*,#11558,.F.);
#16016=ORIENTED_EDGE('',*,*,#11562,.F.);
#16017=ORIENTED_EDGE('',*,*,#11565,.T.);
#16018=ORIENTED_EDGE('',*,*,#11549,.T.);
#16019=ORIENTED_EDGE('',*,*,#11545,.T.);
#16020=ORIENTED_EDGE('',*,*,#11556,.T.);
#16021=ORIENTED_EDGE('',*,*,#11552,.T.);
#16022=ORIENTED_EDGE('',*,*,#11567,.F.);
#16023=ORIENTED_EDGE('',*,*,#11570,.F.);
#16024=ORIENTED_EDGE('',*,*,#11515,.T.);
#16025=ORIENTED_EDGE('',*,*,#11518,.T.);
#16026=ORIENTED_EDGE('',*,*,#11521,.T.);
#16027=ORIENTED_EDGE('',*,*,#11524,.T.);
#16028=ORIENTED_EDGE('',*,*,#11527,.T.);
#16029=ORIENTED_EDGE('',*,*,#11530,.T.);
#16030=ORIENTED_EDGE('',*,*,#11533,.T.);
#16031=ORIENTED_EDGE('',*,*,#11536,.T.);
#16032=ORIENTED_EDGE('',*,*,#11539,.T.);
#16033=ORIENTED_EDGE('',*,*,#11542,.T.);
#16034=ORIENTED_EDGE('',*,*,#11575,.T.);
#16035=ORIENTED_EDGE('',*,*,#11576,.T.);
#16036=ORIENTED_EDGE('',*,*,#11577,.T.);
#16037=ORIENTED_EDGE('',*,*,#11578,.F.);
#16038=ORIENTED_EDGE('',*,*,#11577,.F.);
#16039=ORIENTED_EDGE('',*,*,#11579,.F.);
#16040=ORIENTED_EDGE('',*,*,#11580,.F.);
#16041=ORIENTED_EDGE('',*,*,#11581,.F.);
#16042=ORIENTED_EDGE('',*,*,#11582,.F.);
#16043=ORIENTED_EDGE('',*,*,#11583,.T.);
#16044=ORIENTED_EDGE('',*,*,#11584,.T.);
#16045=ORIENTED_EDGE('',*,*,#11585,.F.);
#16046=ORIENTED_EDGE('',*,*,#11584,.F.);
#16047=ORIENTED_EDGE('',*,*,#11586,.T.);
#16048=ORIENTED_EDGE('',*,*,#11580,.T.);
#16049=ORIENTED_EDGE('',*,*,#11587,.F.);
#16050=ORIENTED_EDGE('',*,*,#11588,.F.);
#16051=ORIENTED_EDGE('',*,*,#11589,.F.);
#16052=ORIENTED_EDGE('',*,*,#11590,.F.);
#16053=ORIENTED_EDGE('',*,*,#11582,.T.);
#16054=ORIENTED_EDGE('',*,*,#11590,.T.);
#16055=ORIENTED_EDGE('',*,*,#11591,.F.);
#16056=ORIENTED_EDGE('',*,*,#11592,.F.);
#16057=ORIENTED_EDGE('',*,*,#11578,.T.);
#16058=ORIENTED_EDGE('',*,*,#11581,.T.);
#16059=ORIENTED_EDGE('',*,*,#11586,.F.);
#16060=ORIENTED_EDGE('',*,*,#11583,.F.);
#16061=ORIENTED_EDGE('',*,*,#11592,.T.);
#16062=ORIENTED_EDGE('',*,*,#11593,.F.);
#16063=ORIENTED_EDGE('',*,*,#11594,.F.);
#16064=ORIENTED_EDGE('',*,*,#11575,.F.);
#16065=ORIENTED_EDGE('',*,*,#11594,.T.);
#16066=ORIENTED_EDGE('',*,*,#11595,.F.);
#16067=ORIENTED_EDGE('',*,*,#11588,.T.);
#16068=ORIENTED_EDGE('',*,*,#11585,.T.);
#16069=ORIENTED_EDGE('',*,*,#11587,.T.);
#16070=ORIENTED_EDGE('',*,*,#11579,.T.);
#16071=ORIENTED_EDGE('',*,*,#11576,.F.);
#16072=ORIENTED_EDGE('',*,*,#11595,.T.);
#16073=ORIENTED_EDGE('',*,*,#11593,.T.);
#16074=ORIENTED_EDGE('',*,*,#11591,.T.);
#16075=ORIENTED_EDGE('',*,*,#11589,.T.);
#16076=ORIENTED_EDGE('',*,*,#11596,.T.);
#16077=ORIENTED_EDGE('',*,*,#11597,.T.);
#16078=ORIENTED_EDGE('',*,*,#11598,.T.);
#16079=ORIENTED_EDGE('',*,*,#11599,.T.);
#16080=ORIENTED_EDGE('',*,*,#11597,.F.);
#16081=ORIENTED_EDGE('',*,*,#11600,.F.);
#16082=ORIENTED_EDGE('',*,*,#11601,.F.);
#16083=ORIENTED_EDGE('',*,*,#11602,.F.);
#16084=ORIENTED_EDGE('',*,*,#11603,.T.);
#16085=ORIENTED_EDGE('',*,*,#11604,.T.);
#16086=ORIENTED_EDGE('',*,*,#11605,.T.);
#16087=ORIENTED_EDGE('',*,*,#11601,.T.);
#16088=ORIENTED_EDGE('',*,*,#11604,.F.);
#16089=ORIENTED_EDGE('',*,*,#11606,.F.);
#16090=ORIENTED_EDGE('',*,*,#11607,.F.);
#16091=ORIENTED_EDGE('',*,*,#11608,.F.);
#16092=ORIENTED_EDGE('',*,*,#11609,.T.);
#16093=ORIENTED_EDGE('',*,*,#11610,.T.);
#16094=ORIENTED_EDGE('',*,*,#11611,.T.);
#16095=ORIENTED_EDGE('',*,*,#11612,.T.);
#16096=ORIENTED_EDGE('',*,*,#11610,.F.);
#16097=ORIENTED_EDGE('',*,*,#11613,.F.);
#16098=ORIENTED_EDGE('',*,*,#11614,.F.);
#16099=ORIENTED_EDGE('',*,*,#11615,.F.);
#16100=ORIENTED_EDGE('',*,*,#11616,.T.);
#16101=ORIENTED_EDGE('',*,*,#11617,.T.);
#16102=ORIENTED_EDGE('',*,*,#11618,.T.);
#16103=ORIENTED_EDGE('',*,*,#11614,.T.);
#16104=ORIENTED_EDGE('',*,*,#11617,.F.);
#16105=ORIENTED_EDGE('',*,*,#11619,.F.);
#16106=ORIENTED_EDGE('',*,*,#11620,.F.);
#16107=ORIENTED_EDGE('',*,*,#11621,.F.);
#16108=ORIENTED_EDGE('',*,*,#11622,.T.);
#16109=ORIENTED_EDGE('',*,*,#11623,.T.);
#16110=ORIENTED_EDGE('',*,*,#11624,.T.);
#16111=ORIENTED_EDGE('',*,*,#11625,.T.);
#16112=ORIENTED_EDGE('',*,*,#11623,.F.);
#16113=ORIENTED_EDGE('',*,*,#11626,.F.);
#16114=ORIENTED_EDGE('',*,*,#11627,.F.);
#16115=ORIENTED_EDGE('',*,*,#11628,.F.);
#16116=ORIENTED_EDGE('',*,*,#11629,.T.);
#16117=ORIENTED_EDGE('',*,*,#11630,.T.);
#16118=ORIENTED_EDGE('',*,*,#11631,.T.);
#16119=ORIENTED_EDGE('',*,*,#11627,.T.);
#16120=ORIENTED_EDGE('',*,*,#11630,.F.);
#16121=ORIENTED_EDGE('',*,*,#11632,.F.);
#16122=ORIENTED_EDGE('',*,*,#11633,.F.);
#16123=ORIENTED_EDGE('',*,*,#11634,.F.);
#16124=ORIENTED_EDGE('',*,*,#11635,.T.);
#16125=ORIENTED_EDGE('',*,*,#11636,.T.);
#16126=ORIENTED_EDGE('',*,*,#11637,.T.);
#16127=ORIENTED_EDGE('',*,*,#11638,.T.);
#16128=ORIENTED_EDGE('',*,*,#11636,.F.);
#16129=ORIENTED_EDGE('',*,*,#11639,.F.);
#16130=ORIENTED_EDGE('',*,*,#11640,.F.);
#16131=ORIENTED_EDGE('',*,*,#11641,.F.);
#16132=ORIENTED_EDGE('',*,*,#11642,.T.);
#16133=ORIENTED_EDGE('',*,*,#11643,.T.);
#16134=ORIENTED_EDGE('',*,*,#11644,.T.);
#16135=ORIENTED_EDGE('',*,*,#11640,.T.);
#16136=ORIENTED_EDGE('',*,*,#11643,.F.);
#16137=ORIENTED_EDGE('',*,*,#11645,.F.);
#16138=ORIENTED_EDGE('',*,*,#11646,.F.);
#16139=ORIENTED_EDGE('',*,*,#11647,.F.);
#16140=ORIENTED_EDGE('',*,*,#11648,.T.);
#16141=ORIENTED_EDGE('',*,*,#11649,.T.);
#16142=ORIENTED_EDGE('',*,*,#11650,.T.);
#16143=ORIENTED_EDGE('',*,*,#11651,.T.);
#16144=ORIENTED_EDGE('',*,*,#11649,.F.);
#16145=ORIENTED_EDGE('',*,*,#11652,.F.);
#16146=ORIENTED_EDGE('',*,*,#11653,.F.);
#16147=ORIENTED_EDGE('',*,*,#11654,.F.);
#16148=ORIENTED_EDGE('',*,*,#11655,.T.);
#16149=ORIENTED_EDGE('',*,*,#11656,.T.);
#16150=ORIENTED_EDGE('',*,*,#11657,.T.);
#16151=ORIENTED_EDGE('',*,*,#11653,.T.);
#16152=ORIENTED_EDGE('',*,*,#11656,.F.);
#16153=ORIENTED_EDGE('',*,*,#11658,.F.);
#16154=ORIENTED_EDGE('',*,*,#11659,.F.);
#16155=ORIENTED_EDGE('',*,*,#11660,.F.);
#16156=ORIENTED_EDGE('',*,*,#11651,.F.);
#16157=ORIENTED_EDGE('',*,*,#11661,.F.);
#16158=ORIENTED_EDGE('',*,*,#11662,.F.);
#16159=ORIENTED_EDGE('',*,*,#11663,.F.);
#16160=ORIENTED_EDGE('',*,*,#11638,.F.);
#16161=ORIENTED_EDGE('',*,*,#11664,.F.);
#16162=ORIENTED_EDGE('',*,*,#11665,.F.);
#16163=ORIENTED_EDGE('',*,*,#11666,.F.);
#16164=ORIENTED_EDGE('',*,*,#11612,.F.);
#16165=ORIENTED_EDGE('',*,*,#11667,.F.);
#16166=ORIENTED_EDGE('',*,*,#11668,.F.);
#16167=ORIENTED_EDGE('',*,*,#11669,.F.);
#16168=ORIENTED_EDGE('',*,*,#11599,.F.);
#16169=ORIENTED_EDGE('',*,*,#11670,.F.);
#16170=ORIENTED_EDGE('',*,*,#11671,.F.);
#16171=ORIENTED_EDGE('',*,*,#11672,.F.);
#16172=ORIENTED_EDGE('',*,*,#11659,.T.);
#16173=ORIENTED_EDGE('',*,*,#11673,.F.);
#16174=ORIENTED_EDGE('',*,*,#11674,.F.);
#16175=ORIENTED_EDGE('',*,*,#11675,.F.);
#16176=ORIENTED_EDGE('',*,*,#11665,.T.);
#16177=ORIENTED_EDGE('',*,*,#11676,.F.);
#16178=ORIENTED_EDGE('',*,*,#11633,.T.);
#16179=ORIENTED_EDGE('',*,*,#11677,.F.);
#16180=ORIENTED_EDGE('',*,*,#11661,.T.);
#16181=ORIENTED_EDGE('',*,*,#11650,.F.);
#16182=ORIENTED_EDGE('',*,*,#11654,.T.);
#16183=ORIENTED_EDGE('',*,*,#11657,.F.);
#16184=ORIENTED_EDGE('',*,*,#11660,.T.);
#16185=ORIENTED_EDGE('',*,*,#11675,.T.);
#16186=ORIENTED_EDGE('',*,*,#11678,.T.);
#16187=ORIENTED_EDGE('',*,*,#11679,.T.);
#16188=ORIENTED_EDGE('',*,*,#11680,.T.);
#16189=ORIENTED_EDGE('',*,*,#11681,.T.);
#16190=ORIENTED_EDGE('',*,*,#11670,.T.);
#16191=ORIENTED_EDGE('',*,*,#11598,.F.);
#16192=ORIENTED_EDGE('',*,*,#11602,.T.);
#16193=ORIENTED_EDGE('',*,*,#11605,.F.);
#16194=ORIENTED_EDGE('',*,*,#11608,.T.);
#16195=ORIENTED_EDGE('',*,*,#11682,.T.);
#16196=ORIENTED_EDGE('',*,*,#11667,.T.);
#16197=ORIENTED_EDGE('',*,*,#11611,.F.);
#16198=ORIENTED_EDGE('',*,*,#11615,.T.);
#16199=ORIENTED_EDGE('',*,*,#11618,.F.);
#16200=ORIENTED_EDGE('',*,*,#11621,.T.);
#16201=ORIENTED_EDGE('',*,*,#11683,.T.);
#16202=ORIENTED_EDGE('',*,*,#11684,.T.);
#16203=ORIENTED_EDGE('',*,*,#11624,.F.);
#16204=ORIENTED_EDGE('',*,*,#11628,.T.);
#16205=ORIENTED_EDGE('',*,*,#11631,.F.);
#16206=ORIENTED_EDGE('',*,*,#11634,.T.);
#16207=ORIENTED_EDGE('',*,*,#11676,.T.);
#16208=ORIENTED_EDGE('',*,*,#11664,.T.);
#16209=ORIENTED_EDGE('',*,*,#11637,.F.);
#16210=ORIENTED_EDGE('',*,*,#11641,.T.);
#16211=ORIENTED_EDGE('',*,*,#11644,.F.);
#16212=ORIENTED_EDGE('',*,*,#11647,.T.);
#16213=ORIENTED_EDGE('',*,*,#11685,.T.);
#16214=ORIENTED_EDGE('',*,*,#11620,.T.);
#16215=ORIENTED_EDGE('',*,*,#11686,.F.);
#16216=ORIENTED_EDGE('',*,*,#11687,.T.);
#16217=ORIENTED_EDGE('',*,*,#11683,.F.);
#16218=ORIENTED_EDGE('',*,*,#11671,.T.);
#16219=ORIENTED_EDGE('',*,*,#11681,.F.);
#16220=ORIENTED_EDGE('',*,*,#11688,.T.);
#16221=ORIENTED_EDGE('',*,*,#11689,.F.);
#16222=ORIENTED_EDGE('',*,*,#11625,.F.);
#16223=ORIENTED_EDGE('',*,*,#11684,.F.);
#16224=ORIENTED_EDGE('',*,*,#11687,.F.);
#16225=ORIENTED_EDGE('',*,*,#11690,.F.);
#16226=ORIENTED_EDGE('',*,*,#11662,.T.);
#16227=ORIENTED_EDGE('',*,*,#11685,.F.);
#16228=ORIENTED_EDGE('',*,*,#11646,.T.);
#16229=ORIENTED_EDGE('',*,*,#11691,.F.);
#16230=ORIENTED_EDGE('',*,*,#11692,.F.);
#16231=ORIENTED_EDGE('',*,*,#11693,.F.);
#16232=ORIENTED_EDGE('',*,*,#11694,.F.);
#16233=ORIENTED_EDGE('',*,*,#11679,.F.);
#16234=ORIENTED_EDGE('',*,*,#11694,.T.);
#16235=ORIENTED_EDGE('',*,*,#11695,.F.);
#16236=ORIENTED_EDGE('',*,*,#11688,.F.);
#16237=ORIENTED_EDGE('',*,*,#11680,.F.);
#16238=ORIENTED_EDGE('',*,*,#11668,.T.);
#16239=ORIENTED_EDGE('',*,*,#11682,.F.);
#16240=ORIENTED_EDGE('',*,*,#11607,.T.);
#16241=ORIENTED_EDGE('',*,*,#11696,.F.);
#16242=ORIENTED_EDGE('',*,*,#11674,.T.);
#16243=ORIENTED_EDGE('',*,*,#11697,.F.);
#16244=ORIENTED_EDGE('',*,*,#11692,.T.);
#16245=ORIENTED_EDGE('',*,*,#11678,.F.);
#16246=ORIENTED_EDGE('',*,*,#11663,.T.);
#16247=ORIENTED_EDGE('',*,*,#11691,.T.);
#16248=ORIENTED_EDGE('',*,*,#11645,.T.);
#16249=ORIENTED_EDGE('',*,*,#11642,.F.);
#16250=ORIENTED_EDGE('',*,*,#11639,.T.);
#16251=ORIENTED_EDGE('',*,*,#11635,.F.);
#16252=ORIENTED_EDGE('',*,*,#11666,.T.);
#16253=ORIENTED_EDGE('',*,*,#11677,.T.);
#16254=ORIENTED_EDGE('',*,*,#11632,.T.);
#16255=ORIENTED_EDGE('',*,*,#11629,.F.);
#16256=ORIENTED_EDGE('',*,*,#11626,.T.);
#16257=ORIENTED_EDGE('',*,*,#11622,.F.);
#16258=ORIENTED_EDGE('',*,*,#11690,.T.);
#16259=ORIENTED_EDGE('',*,*,#11686,.T.);
#16260=ORIENTED_EDGE('',*,*,#11619,.T.);
#16261=ORIENTED_EDGE('',*,*,#11616,.F.);
#16262=ORIENTED_EDGE('',*,*,#11613,.T.);
#16263=ORIENTED_EDGE('',*,*,#11609,.F.);
#16264=ORIENTED_EDGE('',*,*,#11669,.T.);
#16265=ORIENTED_EDGE('',*,*,#11696,.T.);
#16266=ORIENTED_EDGE('',*,*,#11606,.T.);
#16267=ORIENTED_EDGE('',*,*,#11603,.F.);
#16268=ORIENTED_EDGE('',*,*,#11600,.T.);
#16269=ORIENTED_EDGE('',*,*,#11596,.F.);
#16270=ORIENTED_EDGE('',*,*,#11672,.T.);
#16271=ORIENTED_EDGE('',*,*,#11689,.T.);
#16272=ORIENTED_EDGE('',*,*,#11695,.T.);
#16273=ORIENTED_EDGE('',*,*,#11693,.T.);
#16274=ORIENTED_EDGE('',*,*,#11697,.T.);
#16275=ORIENTED_EDGE('',*,*,#11673,.T.);
#16276=ORIENTED_EDGE('',*,*,#11658,.T.);
#16277=ORIENTED_EDGE('',*,*,#11655,.F.);
#16278=ORIENTED_EDGE('',*,*,#11652,.T.);
#16279=ORIENTED_EDGE('',*,*,#11648,.F.);
#16280=ORIENTED_EDGE('',*,*,#11698,.T.);
#16281=ORIENTED_EDGE('',*,*,#11699,.T.);
#16282=ORIENTED_EDGE('',*,*,#11699,.F.);
#16283=ORIENTED_EDGE('',*,*,#11700,.T.);
#16284=ORIENTED_EDGE('',*,*,#11701,.F.);
#16285=ORIENTED_EDGE('',*,*,#11700,.F.);
#16286=ORIENTED_EDGE('',*,*,#11702,.F.);
#16287=ORIENTED_EDGE('',*,*,#11703,.T.);
#16288=ORIENTED_EDGE('',*,*,#11698,.F.);
#16289=ORIENTED_EDGE('',*,*,#11703,.F.);
#16290=ORIENTED_EDGE('',*,*,#11702,.T.);
#16291=ORIENTED_EDGE('',*,*,#11701,.T.);
#16292=ORIENTED_EDGE('',*,*,#11704,.T.);
#16293=ORIENTED_EDGE('',*,*,#11705,.T.);
#16294=ORIENTED_EDGE('',*,*,#11706,.T.);
#16295=ORIENTED_EDGE('',*,*,#11707,.F.);
#16296=ORIENTED_EDGE('',*,*,#11706,.F.);
#16297=ORIENTED_EDGE('',*,*,#11708,.F.);
#16298=ORIENTED_EDGE('',*,*,#11709,.F.);
#16299=ORIENTED_EDGE('',*,*,#11710,.F.);
#16300=ORIENTED_EDGE('',*,*,#11707,.T.);
#16301=ORIENTED_EDGE('',*,*,#11710,.T.);
#16302=ORIENTED_EDGE('',*,*,#11711,.F.);
#16303=ORIENTED_EDGE('',*,*,#11712,.F.);
#16304=ORIENTED_EDGE('',*,*,#11713,.T.);
#16305=ORIENTED_EDGE('',*,*,#11714,.F.);
#16306=ORIENTED_EDGE('',*,*,#11715,.T.);
#16307=ORIENTED_EDGE('',*,*,#11716,.F.);
#16308=ORIENTED_EDGE('',*,*,#11712,.T.);
#16309=ORIENTED_EDGE('',*,*,#11717,.T.);
#16310=ORIENTED_EDGE('',*,*,#11718,.F.);
#16311=ORIENTED_EDGE('',*,*,#11718,.T.);
#16312=ORIENTED_EDGE('',*,*,#11719,.T.);
#16313=ORIENTED_EDGE('',*,*,#11708,.T.);
#16314=ORIENTED_EDGE('',*,*,#11705,.F.);
#16315=ORIENTED_EDGE('',*,*,#11720,.T.);
#16316=ORIENTED_EDGE('',*,*,#11721,.F.);
#16317=ORIENTED_EDGE('',*,*,#11722,.F.);
#16318=ORIENTED_EDGE('',*,*,#11717,.F.);
#16319=ORIENTED_EDGE('',*,*,#11711,.T.);
#16320=ORIENTED_EDGE('',*,*,#11709,.T.);
#16321=ORIENTED_EDGE('',*,*,#11719,.F.);
#16322=ORIENTED_EDGE('',*,*,#11715,.F.);
#16323=ORIENTED_EDGE('',*,*,#11723,.F.);
#16324=ORIENTED_EDGE('',*,*,#11720,.F.);
#16325=ORIENTED_EDGE('',*,*,#11704,.F.);
#16326=ORIENTED_EDGE('',*,*,#11722,.T.);
#16327=ORIENTED_EDGE('',*,*,#11724,.F.);
#16328=ORIENTED_EDGE('',*,*,#11713,.F.);
#16329=ORIENTED_EDGE('',*,*,#11716,.T.);
#16330=ORIENTED_EDGE('',*,*,#11714,.T.);
#16331=ORIENTED_EDGE('',*,*,#11724,.T.);
#16332=ORIENTED_EDGE('',*,*,#11721,.T.);
#16333=ORIENTED_EDGE('',*,*,#11723,.T.);
#16334=ORIENTED_EDGE('',*,*,#11725,.F.);
#16335=ORIENTED_EDGE('',*,*,#11726,.F.);
#16336=ORIENTED_EDGE('',*,*,#11727,.F.);
#16337=ORIENTED_EDGE('',*,*,#11728,.F.);
#16338=ORIENTED_EDGE('',*,*,#11729,.F.);
#16339=ORIENTED_EDGE('',*,*,#11730,.F.);
#16340=ORIENTED_EDGE('',*,*,#11731,.F.);
#16341=ORIENTED_EDGE('',*,*,#11732,.F.);
#16342=ORIENTED_EDGE('',*,*,#11733,.F.);
#16343=ORIENTED_EDGE('',*,*,#11734,.F.);
#16344=ORIENTED_EDGE('',*,*,#11735,.F.);
#16345=ORIENTED_EDGE('',*,*,#11736,.F.);
#16346=ORIENTED_EDGE('',*,*,#11737,.F.);
#16347=ORIENTED_EDGE('',*,*,#11738,.F.);
#16348=ORIENTED_EDGE('',*,*,#11739,.F.);
#16349=ORIENTED_EDGE('',*,*,#11740,.F.);
#16350=ORIENTED_EDGE('',*,*,#11741,.F.);
#16351=ORIENTED_EDGE('',*,*,#11742,.F.);
#16352=ORIENTED_EDGE('',*,*,#11743,.F.);
#16353=ORIENTED_EDGE('',*,*,#11744,.F.);
#16354=ORIENTED_EDGE('',*,*,#11745,.F.);
#16355=ORIENTED_EDGE('',*,*,#11746,.F.);
#16356=ORIENTED_EDGE('',*,*,#11747,.F.);
#16357=ORIENTED_EDGE('',*,*,#11748,.F.);
#16358=ORIENTED_EDGE('',*,*,#11749,.F.);
#16359=ORIENTED_EDGE('',*,*,#11750,.F.);
#16360=ORIENTED_EDGE('',*,*,#11751,.F.);
#16361=ORIENTED_EDGE('',*,*,#11752,.F.);
#16362=ORIENTED_EDGE('',*,*,#11753,.F.);
#16363=ORIENTED_EDGE('',*,*,#11754,.F.);
#16364=ORIENTED_EDGE('',*,*,#11755,.F.);
#16365=ORIENTED_EDGE('',*,*,#11756,.F.);
#16366=ORIENTED_EDGE('',*,*,#11757,.F.);
#16367=ORIENTED_EDGE('',*,*,#11758,.F.);
#16368=ORIENTED_EDGE('',*,*,#11759,.F.);
#16369=ORIENTED_EDGE('',*,*,#11760,.F.);
#16370=ORIENTED_EDGE('',*,*,#11761,.F.);
#16371=ORIENTED_EDGE('',*,*,#11762,.F.);
#16372=ORIENTED_EDGE('',*,*,#11763,.F.);
#16373=ORIENTED_EDGE('',*,*,#11764,.F.);
#16374=ORIENTED_EDGE('',*,*,#11765,.F.);
#16375=ORIENTED_EDGE('',*,*,#11766,.F.);
#16376=ORIENTED_EDGE('',*,*,#11767,.F.);
#16377=ORIENTED_EDGE('',*,*,#11768,.F.);
#16378=ORIENTED_EDGE('',*,*,#11769,.F.);
#16379=ORIENTED_EDGE('',*,*,#11770,.F.);
#16380=ORIENTED_EDGE('',*,*,#11771,.F.);
#16381=ORIENTED_EDGE('',*,*,#11772,.F.);
#16382=ORIENTED_EDGE('',*,*,#11773,.F.);
#16383=ORIENTED_EDGE('',*,*,#11774,.F.);
#16384=ORIENTED_EDGE('',*,*,#11775,.F.);
#16385=ORIENTED_EDGE('',*,*,#11776,.F.);
#16386=ORIENTED_EDGE('',*,*,#11777,.F.);
#16387=ORIENTED_EDGE('',*,*,#11778,.F.);
#16388=ORIENTED_EDGE('',*,*,#11779,.F.);
#16389=ORIENTED_EDGE('',*,*,#11780,.F.);
#16390=ORIENTED_EDGE('',*,*,#11781,.F.);
#16391=ORIENTED_EDGE('',*,*,#11782,.F.);
#16392=ORIENTED_EDGE('',*,*,#11783,.F.);
#16393=ORIENTED_EDGE('',*,*,#11784,.F.);
#16394=ORIENTED_EDGE('',*,*,#11785,.F.);
#16395=ORIENTED_EDGE('',*,*,#11786,.F.);
#16396=ORIENTED_EDGE('',*,*,#11787,.F.);
#16397=ORIENTED_EDGE('',*,*,#11788,.F.);
#16398=ORIENTED_EDGE('',*,*,#11789,.F.);
#16399=ORIENTED_EDGE('',*,*,#11790,.F.);
#16400=ORIENTED_EDGE('',*,*,#11791,.F.);
#16401=ORIENTED_EDGE('',*,*,#11792,.F.);
#16402=ORIENTED_EDGE('',*,*,#11793,.F.);
#16403=ORIENTED_EDGE('',*,*,#11794,.F.);
#16404=ORIENTED_EDGE('',*,*,#11795,.F.);
#16405=ORIENTED_EDGE('',*,*,#11796,.F.);
#16406=ORIENTED_EDGE('',*,*,#11797,.F.);
#16407=ORIENTED_EDGE('',*,*,#11798,.F.);
#16408=ORIENTED_EDGE('',*,*,#11799,.F.);
#16409=ORIENTED_EDGE('',*,*,#11800,.F.);
#16410=ORIENTED_EDGE('',*,*,#11801,.F.);
#16411=ORIENTED_EDGE('',*,*,#11802,.F.);
#16412=ORIENTED_EDGE('',*,*,#11803,.F.);
#16413=ORIENTED_EDGE('',*,*,#11804,.F.);
#16414=ORIENTED_EDGE('',*,*,#11805,.F.);
#16415=ORIENTED_EDGE('',*,*,#11806,.F.);
#16416=ORIENTED_EDGE('',*,*,#11807,.F.);
#16417=ORIENTED_EDGE('',*,*,#11808,.F.);
#16418=ORIENTED_EDGE('',*,*,#11809,.F.);
#16419=ORIENTED_EDGE('',*,*,#11810,.F.);
#16420=ORIENTED_EDGE('',*,*,#11811,.F.);
#16421=ORIENTED_EDGE('',*,*,#11812,.F.);
#16422=ORIENTED_EDGE('',*,*,#11813,.F.);
#16423=ORIENTED_EDGE('',*,*,#11814,.F.);
#16424=ORIENTED_EDGE('',*,*,#11815,.F.);
#16425=ORIENTED_EDGE('',*,*,#11816,.F.);
#16426=ORIENTED_EDGE('',*,*,#11817,.F.);
#16427=ORIENTED_EDGE('',*,*,#11818,.F.);
#16428=ORIENTED_EDGE('',*,*,#11819,.F.);
#16429=ORIENTED_EDGE('',*,*,#11820,.F.);
#16430=ORIENTED_EDGE('',*,*,#11821,.F.);
#16431=ORIENTED_EDGE('',*,*,#11822,.F.);
#16432=ORIENTED_EDGE('',*,*,#11823,.F.);
#16433=ORIENTED_EDGE('',*,*,#11824,.F.);
#16434=ORIENTED_EDGE('',*,*,#11825,.F.);
#16435=ORIENTED_EDGE('',*,*,#11826,.F.);
#16436=ORIENTED_EDGE('',*,*,#11827,.F.);
#16437=ORIENTED_EDGE('',*,*,#11828,.F.);
#16438=ORIENTED_EDGE('',*,*,#11829,.F.);
#16439=ORIENTED_EDGE('',*,*,#11830,.F.);
#16440=ORIENTED_EDGE('',*,*,#11831,.F.);
#16441=ORIENTED_EDGE('',*,*,#11832,.F.);
#16442=ORIENTED_EDGE('',*,*,#11833,.F.);
#16443=ORIENTED_EDGE('',*,*,#11834,.F.);
#16444=ORIENTED_EDGE('',*,*,#11835,.F.);
#16445=ORIENTED_EDGE('',*,*,#11836,.F.);
#16446=ORIENTED_EDGE('',*,*,#11837,.F.);
#16447=ORIENTED_EDGE('',*,*,#11838,.F.);
#16448=ORIENTED_EDGE('',*,*,#11839,.F.);
#16449=ORIENTED_EDGE('',*,*,#11840,.F.);
#16450=ORIENTED_EDGE('',*,*,#11841,.F.);
#16451=ORIENTED_EDGE('',*,*,#11842,.F.);
#16452=ORIENTED_EDGE('',*,*,#11843,.F.);
#16453=ORIENTED_EDGE('',*,*,#11844,.F.);
#16454=ORIENTED_EDGE('',*,*,#11845,.F.);
#16455=ORIENTED_EDGE('',*,*,#11846,.F.);
#16456=ORIENTED_EDGE('',*,*,#11847,.F.);
#16457=ORIENTED_EDGE('',*,*,#11848,.F.);
#16458=ORIENTED_EDGE('',*,*,#11849,.F.);
#16459=ORIENTED_EDGE('',*,*,#11850,.F.);
#16460=ORIENTED_EDGE('',*,*,#11851,.F.);
#16461=ORIENTED_EDGE('',*,*,#11852,.F.);
#16462=ORIENTED_EDGE('',*,*,#11853,.F.);
#16463=ORIENTED_EDGE('',*,*,#11854,.F.);
#16464=ORIENTED_EDGE('',*,*,#11855,.F.);
#16465=ORIENTED_EDGE('',*,*,#11856,.F.);
#16466=ORIENTED_EDGE('',*,*,#11857,.F.);
#16467=ORIENTED_EDGE('',*,*,#11858,.F.);
#16468=ORIENTED_EDGE('',*,*,#11859,.F.);
#16469=ORIENTED_EDGE('',*,*,#11860,.F.);
#16470=ORIENTED_EDGE('',*,*,#11861,.F.);
#16471=ORIENTED_EDGE('',*,*,#11862,.F.);
#16472=ORIENTED_EDGE('',*,*,#11863,.F.);
#16473=ORIENTED_EDGE('',*,*,#11864,.F.);
#16474=ORIENTED_EDGE('',*,*,#11865,.F.);
#16475=ORIENTED_EDGE('',*,*,#11866,.F.);
#16476=ORIENTED_EDGE('',*,*,#11867,.F.);
#16477=ORIENTED_EDGE('',*,*,#11868,.F.);
#16478=ORIENTED_EDGE('',*,*,#11869,.F.);
#16479=ORIENTED_EDGE('',*,*,#11870,.F.);
#16480=ORIENTED_EDGE('',*,*,#11871,.F.);
#16481=ORIENTED_EDGE('',*,*,#11872,.F.);
#16482=ORIENTED_EDGE('',*,*,#11873,.F.);
#16483=ORIENTED_EDGE('',*,*,#11874,.F.);
#16484=ORIENTED_EDGE('',*,*,#11875,.F.);
#16485=ORIENTED_EDGE('',*,*,#11876,.F.);
#16486=ORIENTED_EDGE('',*,*,#11877,.F.);
#16487=ORIENTED_EDGE('',*,*,#11878,.F.);
#16488=ORIENTED_EDGE('',*,*,#11879,.F.);
#16489=ORIENTED_EDGE('',*,*,#11880,.F.);
#16490=ORIENTED_EDGE('',*,*,#11881,.F.);
#16491=ORIENTED_EDGE('',*,*,#11882,.F.);
#16492=ORIENTED_EDGE('',*,*,#11883,.F.);
#16493=ORIENTED_EDGE('',*,*,#11884,.F.);
#16494=ORIENTED_EDGE('',*,*,#11885,.F.);
#16495=ORIENTED_EDGE('',*,*,#11886,.F.);
#16496=ORIENTED_EDGE('',*,*,#11887,.F.);
#16497=ORIENTED_EDGE('',*,*,#11888,.F.);
#16498=ORIENTED_EDGE('',*,*,#11889,.F.);
#16499=ORIENTED_EDGE('',*,*,#11890,.F.);
#16500=ORIENTED_EDGE('',*,*,#11891,.F.);
#16501=ORIENTED_EDGE('',*,*,#11892,.F.);
#16502=ORIENTED_EDGE('',*,*,#11893,.F.);
#16503=ORIENTED_EDGE('',*,*,#11894,.F.);
#16504=ORIENTED_EDGE('',*,*,#11895,.F.);
#16505=ORIENTED_EDGE('',*,*,#11896,.F.);
#16506=ORIENTED_EDGE('',*,*,#11897,.F.);
#16507=ORIENTED_EDGE('',*,*,#11898,.F.);
#16508=ORIENTED_EDGE('',*,*,#11899,.F.);
#16509=ORIENTED_EDGE('',*,*,#11900,.F.);
#16510=ORIENTED_EDGE('',*,*,#11726,.T.);
#16511=ORIENTED_EDGE('',*,*,#11901,.T.);
#16512=ORIENTED_EDGE('',*,*,#11902,.T.);
#16513=ORIENTED_EDGE('',*,*,#11903,.T.);
#16514=ORIENTED_EDGE('',*,*,#11898,.T.);
#16515=ORIENTED_EDGE('',*,*,#11904,.T.);
#16516=ORIENTED_EDGE('',*,*,#11894,.T.);
#16517=ORIENTED_EDGE('',*,*,#11905,.T.);
#16518=ORIENTED_EDGE('',*,*,#11890,.T.);
#16519=ORIENTED_EDGE('',*,*,#11906,.T.);
#16520=ORIENTED_EDGE('',*,*,#11886,.T.);
#16521=ORIENTED_EDGE('',*,*,#11907,.T.);
#16522=ORIENTED_EDGE('',*,*,#11882,.T.);
#16523=ORIENTED_EDGE('',*,*,#11908,.T.);
#16524=ORIENTED_EDGE('',*,*,#11878,.T.);
#16525=ORIENTED_EDGE('',*,*,#11909,.T.);
#16526=ORIENTED_EDGE('',*,*,#11874,.T.);
#16527=ORIENTED_EDGE('',*,*,#11910,.T.);
#16528=ORIENTED_EDGE('',*,*,#11870,.T.);
#16529=ORIENTED_EDGE('',*,*,#11911,.T.);
#16530=ORIENTED_EDGE('',*,*,#11866,.T.);
#16531=ORIENTED_EDGE('',*,*,#11912,.T.);
#16532=ORIENTED_EDGE('',*,*,#11862,.T.);
#16533=ORIENTED_EDGE('',*,*,#11913,.T.);
#16534=ORIENTED_EDGE('',*,*,#11858,.T.);
#16535=ORIENTED_EDGE('',*,*,#11914,.T.);
#16536=ORIENTED_EDGE('',*,*,#11854,.T.);
#16537=ORIENTED_EDGE('',*,*,#11915,.T.);
#16538=ORIENTED_EDGE('',*,*,#11850,.T.);
#16539=ORIENTED_EDGE('',*,*,#11916,.T.);
#16540=ORIENTED_EDGE('',*,*,#11846,.T.);
#16541=ORIENTED_EDGE('',*,*,#11917,.T.);
#16542=ORIENTED_EDGE('',*,*,#11842,.T.);
#16543=ORIENTED_EDGE('',*,*,#11918,.T.);
#16544=ORIENTED_EDGE('',*,*,#11838,.T.);
#16545=ORIENTED_EDGE('',*,*,#11919,.T.);
#16546=ORIENTED_EDGE('',*,*,#11834,.T.);
#16547=ORIENTED_EDGE('',*,*,#11920,.T.);
#16548=ORIENTED_EDGE('',*,*,#11830,.T.);
#16549=ORIENTED_EDGE('',*,*,#11921,.T.);
#16550=ORIENTED_EDGE('',*,*,#11826,.T.);
#16551=ORIENTED_EDGE('',*,*,#11922,.T.);
#16552=ORIENTED_EDGE('',*,*,#11822,.T.);
#16553=ORIENTED_EDGE('',*,*,#11923,.T.);
#16554=ORIENTED_EDGE('',*,*,#11818,.T.);
#16555=ORIENTED_EDGE('',*,*,#11924,.T.);
#16556=ORIENTED_EDGE('',*,*,#11814,.T.);
#16557=ORIENTED_EDGE('',*,*,#11925,.T.);
#16558=ORIENTED_EDGE('',*,*,#11810,.T.);
#16559=ORIENTED_EDGE('',*,*,#11926,.T.);
#16560=ORIENTED_EDGE('',*,*,#11806,.T.);
#16561=ORIENTED_EDGE('',*,*,#11927,.T.);
#16562=ORIENTED_EDGE('',*,*,#11802,.T.);
#16563=ORIENTED_EDGE('',*,*,#11928,.T.);
#16564=ORIENTED_EDGE('',*,*,#11798,.T.);
#16565=ORIENTED_EDGE('',*,*,#11929,.T.);
#16566=ORIENTED_EDGE('',*,*,#11794,.T.);
#16567=ORIENTED_EDGE('',*,*,#11930,.T.);
#16568=ORIENTED_EDGE('',*,*,#11790,.T.);
#16569=ORIENTED_EDGE('',*,*,#11931,.T.);
#16570=ORIENTED_EDGE('',*,*,#11786,.T.);
#16571=ORIENTED_EDGE('',*,*,#11932,.T.);
#16572=ORIENTED_EDGE('',*,*,#11782,.T.);
#16573=ORIENTED_EDGE('',*,*,#11933,.T.);
#16574=ORIENTED_EDGE('',*,*,#11778,.T.);
#16575=ORIENTED_EDGE('',*,*,#11934,.T.);
#16576=ORIENTED_EDGE('',*,*,#11774,.T.);
#16577=ORIENTED_EDGE('',*,*,#11935,.T.);
#16578=ORIENTED_EDGE('',*,*,#11770,.T.);
#16579=ORIENTED_EDGE('',*,*,#11936,.T.);
#16580=ORIENTED_EDGE('',*,*,#11766,.T.);
#16581=ORIENTED_EDGE('',*,*,#11937,.T.);
#16582=ORIENTED_EDGE('',*,*,#11762,.T.);
#16583=ORIENTED_EDGE('',*,*,#11938,.T.);
#16584=ORIENTED_EDGE('',*,*,#11758,.T.);
#16585=ORIENTED_EDGE('',*,*,#11939,.T.);
#16586=ORIENTED_EDGE('',*,*,#11754,.T.);
#16587=ORIENTED_EDGE('',*,*,#11940,.T.);
#16588=ORIENTED_EDGE('',*,*,#11750,.T.);
#16589=ORIENTED_EDGE('',*,*,#11941,.T.);
#16590=ORIENTED_EDGE('',*,*,#11746,.T.);
#16591=ORIENTED_EDGE('',*,*,#11942,.T.);
#16592=ORIENTED_EDGE('',*,*,#11742,.T.);
#16593=ORIENTED_EDGE('',*,*,#11943,.T.);
#16594=ORIENTED_EDGE('',*,*,#11738,.T.);
#16595=ORIENTED_EDGE('',*,*,#11944,.T.);
#16596=ORIENTED_EDGE('',*,*,#11734,.T.);
#16597=ORIENTED_EDGE('',*,*,#11945,.T.);
#16598=ORIENTED_EDGE('',*,*,#11730,.T.);
#16599=ORIENTED_EDGE('',*,*,#11946,.T.);
#16600=ORIENTED_EDGE('',*,*,#11947,.T.);
#16601=ORIENTED_EDGE('',*,*,#11725,.T.);
#16602=ORIENTED_EDGE('',*,*,#11948,.T.);
#16603=ORIENTED_EDGE('',*,*,#11949,.T.);
#16604=ORIENTED_EDGE('',*,*,#11901,.F.);
#16605=ORIENTED_EDGE('',*,*,#11899,.T.);
#16606=ORIENTED_EDGE('',*,*,#11903,.F.);
#16607=ORIENTED_EDGE('',*,*,#11950,.T.);
#16608=ORIENTED_EDGE('',*,*,#11951,.T.);
#16609=ORIENTED_EDGE('',*,*,#11895,.T.);
#16610=ORIENTED_EDGE('',*,*,#11904,.F.);
#16611=ORIENTED_EDGE('',*,*,#11897,.T.);
#16612=ORIENTED_EDGE('',*,*,#11952,.T.);
#16613=ORIENTED_EDGE('',*,*,#11891,.T.);
#16614=ORIENTED_EDGE('',*,*,#11905,.F.);
#16615=ORIENTED_EDGE('',*,*,#11893,.T.);
#16616=ORIENTED_EDGE('',*,*,#11953,.T.);
#16617=ORIENTED_EDGE('',*,*,#11887,.T.);
#16618=ORIENTED_EDGE('',*,*,#11906,.F.);
#16619=ORIENTED_EDGE('',*,*,#11889,.T.);
#16620=ORIENTED_EDGE('',*,*,#11954,.T.);
#16621=ORIENTED_EDGE('',*,*,#11883,.T.);
#16622=ORIENTED_EDGE('',*,*,#11907,.F.);
#16623=ORIENTED_EDGE('',*,*,#11885,.T.);
#16624=ORIENTED_EDGE('',*,*,#11955,.T.);
#16625=ORIENTED_EDGE('',*,*,#11879,.T.);
#16626=ORIENTED_EDGE('',*,*,#11908,.F.);
#16627=ORIENTED_EDGE('',*,*,#11881,.T.);
#16628=ORIENTED_EDGE('',*,*,#11956,.T.);
#16629=ORIENTED_EDGE('',*,*,#11875,.T.);
#16630=ORIENTED_EDGE('',*,*,#11909,.F.);
#16631=ORIENTED_EDGE('',*,*,#11877,.T.);
#16632=ORIENTED_EDGE('',*,*,#11957,.T.);
#16633=ORIENTED_EDGE('',*,*,#11871,.T.);
#16634=ORIENTED_EDGE('',*,*,#11910,.F.);
#16635=ORIENTED_EDGE('',*,*,#11873,.T.);
#16636=ORIENTED_EDGE('',*,*,#11958,.T.);
#16637=ORIENTED_EDGE('',*,*,#11867,.T.);
#16638=ORIENTED_EDGE('',*,*,#11911,.F.);
#16639=ORIENTED_EDGE('',*,*,#11869,.T.);
#16640=ORIENTED_EDGE('',*,*,#11959,.T.);
#16641=ORIENTED_EDGE('',*,*,#11863,.T.);
#16642=ORIENTED_EDGE('',*,*,#11912,.F.);
#16643=ORIENTED_EDGE('',*,*,#11865,.T.);
#16644=ORIENTED_EDGE('',*,*,#11960,.T.);
#16645=ORIENTED_EDGE('',*,*,#11859,.T.);
#16646=ORIENTED_EDGE('',*,*,#11913,.F.);
#16647=ORIENTED_EDGE('',*,*,#11861,.T.);
#16648=ORIENTED_EDGE('',*,*,#11961,.T.);
#16649=ORIENTED_EDGE('',*,*,#11855,.T.);
#16650=ORIENTED_EDGE('',*,*,#11914,.F.);
#16651=ORIENTED_EDGE('',*,*,#11857,.T.);
#16652=ORIENTED_EDGE('',*,*,#11962,.T.);
#16653=ORIENTED_EDGE('',*,*,#11851,.T.);
#16654=ORIENTED_EDGE('',*,*,#11915,.F.);
#16655=ORIENTED_EDGE('',*,*,#11853,.T.);
#16656=ORIENTED_EDGE('',*,*,#11963,.T.);
#16657=ORIENTED_EDGE('',*,*,#11847,.T.);
#16658=ORIENTED_EDGE('',*,*,#11916,.F.);
#16659=ORIENTED_EDGE('',*,*,#11849,.T.);
#16660=ORIENTED_EDGE('',*,*,#11964,.T.);
#16661=ORIENTED_EDGE('',*,*,#11843,.T.);
#16662=ORIENTED_EDGE('',*,*,#11917,.F.);
#16663=ORIENTED_EDGE('',*,*,#11845,.T.);
#16664=ORIENTED_EDGE('',*,*,#11965,.T.);
#16665=ORIENTED_EDGE('',*,*,#11839,.T.);
#16666=ORIENTED_EDGE('',*,*,#11918,.F.);
#16667=ORIENTED_EDGE('',*,*,#11841,.T.);
#16668=ORIENTED_EDGE('',*,*,#11966,.T.);
#16669=ORIENTED_EDGE('',*,*,#11835,.T.);
#16670=ORIENTED_EDGE('',*,*,#11919,.F.);
#16671=ORIENTED_EDGE('',*,*,#11837,.T.);
#16672=ORIENTED_EDGE('',*,*,#11967,.T.);
#16673=ORIENTED_EDGE('',*,*,#11831,.T.);
#16674=ORIENTED_EDGE('',*,*,#11920,.F.);
#16675=ORIENTED_EDGE('',*,*,#11833,.T.);
#16676=ORIENTED_EDGE('',*,*,#11968,.T.);
#16677=ORIENTED_EDGE('',*,*,#11827,.T.);
#16678=ORIENTED_EDGE('',*,*,#11921,.F.);
#16679=ORIENTED_EDGE('',*,*,#11829,.T.);
#16680=ORIENTED_EDGE('',*,*,#11969,.T.);
#16681=ORIENTED_EDGE('',*,*,#11823,.T.);
#16682=ORIENTED_EDGE('',*,*,#11922,.F.);
#16683=ORIENTED_EDGE('',*,*,#11825,.T.);
#16684=ORIENTED_EDGE('',*,*,#11970,.T.);
#16685=ORIENTED_EDGE('',*,*,#11819,.T.);
#16686=ORIENTED_EDGE('',*,*,#11923,.F.);
#16687=ORIENTED_EDGE('',*,*,#11821,.T.);
#16688=ORIENTED_EDGE('',*,*,#11971,.T.);
#16689=ORIENTED_EDGE('',*,*,#11815,.T.);
#16690=ORIENTED_EDGE('',*,*,#11924,.F.);
#16691=ORIENTED_EDGE('',*,*,#11817,.T.);
#16692=ORIENTED_EDGE('',*,*,#11972,.T.);
#16693=ORIENTED_EDGE('',*,*,#11811,.T.);
#16694=ORIENTED_EDGE('',*,*,#11925,.F.);
#16695=ORIENTED_EDGE('',*,*,#11813,.T.);
#16696=ORIENTED_EDGE('',*,*,#11973,.T.);
#16697=ORIENTED_EDGE('',*,*,#11807,.T.);
#16698=ORIENTED_EDGE('',*,*,#11926,.F.);
#16699=ORIENTED_EDGE('',*,*,#11809,.T.);
#16700=ORIENTED_EDGE('',*,*,#11974,.T.);
#16701=ORIENTED_EDGE('',*,*,#11803,.T.);
#16702=ORIENTED_EDGE('',*,*,#11927,.F.);
#16703=ORIENTED_EDGE('',*,*,#11805,.T.);
#16704=ORIENTED_EDGE('',*,*,#11975,.T.);
#16705=ORIENTED_EDGE('',*,*,#11799,.T.);
#16706=ORIENTED_EDGE('',*,*,#11928,.F.);
#16707=ORIENTED_EDGE('',*,*,#11801,.T.);
#16708=ORIENTED_EDGE('',*,*,#11976,.T.);
#16709=ORIENTED_EDGE('',*,*,#11795,.T.);
#16710=ORIENTED_EDGE('',*,*,#11929,.F.);
#16711=ORIENTED_EDGE('',*,*,#11797,.T.);
#16712=ORIENTED_EDGE('',*,*,#11977,.T.);
#16713=ORIENTED_EDGE('',*,*,#11791,.T.);
#16714=ORIENTED_EDGE('',*,*,#11930,.F.);
#16715=ORIENTED_EDGE('',*,*,#11793,.T.);
#16716=ORIENTED_EDGE('',*,*,#11978,.T.);
#16717=ORIENTED_EDGE('',*,*,#11787,.T.);
#16718=ORIENTED_EDGE('',*,*,#11931,.F.);
#16719=ORIENTED_EDGE('',*,*,#11789,.T.);
#16720=ORIENTED_EDGE('',*,*,#11979,.T.);
#16721=ORIENTED_EDGE('',*,*,#11783,.T.);
#16722=ORIENTED_EDGE('',*,*,#11932,.F.);
#16723=ORIENTED_EDGE('',*,*,#11785,.T.);
#16724=ORIENTED_EDGE('',*,*,#11980,.T.);
#16725=ORIENTED_EDGE('',*,*,#11779,.T.);
#16726=ORIENTED_EDGE('',*,*,#11933,.F.);
#16727=ORIENTED_EDGE('',*,*,#11781,.T.);
#16728=ORIENTED_EDGE('',*,*,#11981,.T.);
#16729=ORIENTED_EDGE('',*,*,#11775,.T.);
#16730=ORIENTED_EDGE('',*,*,#11934,.F.);
#16731=ORIENTED_EDGE('',*,*,#11777,.T.);
#16732=ORIENTED_EDGE('',*,*,#11982,.T.);
#16733=ORIENTED_EDGE('',*,*,#11771,.T.);
#16734=ORIENTED_EDGE('',*,*,#11935,.F.);
#16735=ORIENTED_EDGE('',*,*,#11773,.T.);
#16736=ORIENTED_EDGE('',*,*,#11983,.T.);
#16737=ORIENTED_EDGE('',*,*,#11767,.T.);
#16738=ORIENTED_EDGE('',*,*,#11936,.F.);
#16739=ORIENTED_EDGE('',*,*,#11769,.T.);
#16740=ORIENTED_EDGE('',*,*,#11984,.T.);
#16741=ORIENTED_EDGE('',*,*,#11763,.T.);
#16742=ORIENTED_EDGE('',*,*,#11937,.F.);
#16743=ORIENTED_EDGE('',*,*,#11765,.T.);
#16744=ORIENTED_EDGE('',*,*,#11985,.T.);
#16745=ORIENTED_EDGE('',*,*,#11759,.T.);
#16746=ORIENTED_EDGE('',*,*,#11938,.F.);
#16747=ORIENTED_EDGE('',*,*,#11761,.T.);
#16748=ORIENTED_EDGE('',*,*,#11986,.T.);
#16749=ORIENTED_EDGE('',*,*,#11755,.T.);
#16750=ORIENTED_EDGE('',*,*,#11939,.F.);
#16751=ORIENTED_EDGE('',*,*,#11757,.T.);
#16752=ORIENTED_EDGE('',*,*,#11987,.T.);
#16753=ORIENTED_EDGE('',*,*,#11751,.T.);
#16754=ORIENTED_EDGE('',*,*,#11940,.F.);
#16755=ORIENTED_EDGE('',*,*,#11753,.T.);
#16756=ORIENTED_EDGE('',*,*,#11988,.T.);
#16757=ORIENTED_EDGE('',*,*,#11747,.T.);
#16758=ORIENTED_EDGE('',*,*,#11941,.F.);
#16759=ORIENTED_EDGE('',*,*,#11749,.T.);
#16760=ORIENTED_EDGE('',*,*,#11989,.T.);
#16761=ORIENTED_EDGE('',*,*,#11743,.T.);
#16762=ORIENTED_EDGE('',*,*,#11942,.F.);
#16763=ORIENTED_EDGE('',*,*,#11745,.T.);
#16764=ORIENTED_EDGE('',*,*,#11990,.T.);
#16765=ORIENTED_EDGE('',*,*,#11739,.T.);
#16766=ORIENTED_EDGE('',*,*,#11943,.F.);
#16767=ORIENTED_EDGE('',*,*,#11741,.T.);
#16768=ORIENTED_EDGE('',*,*,#11991,.T.);
#16769=ORIENTED_EDGE('',*,*,#11735,.T.);
#16770=ORIENTED_EDGE('',*,*,#11944,.F.);
#16771=ORIENTED_EDGE('',*,*,#11737,.T.);
#16772=ORIENTED_EDGE('',*,*,#11992,.T.);
#16773=ORIENTED_EDGE('',*,*,#11731,.T.);
#16774=ORIENTED_EDGE('',*,*,#11945,.F.);
#16775=ORIENTED_EDGE('',*,*,#11733,.T.);
#16776=ORIENTED_EDGE('',*,*,#11993,.T.);
#16777=ORIENTED_EDGE('',*,*,#11950,.F.);
#16778=ORIENTED_EDGE('',*,*,#11902,.F.);
#16779=ORIENTED_EDGE('',*,*,#11949,.F.);
#16780=ORIENTED_EDGE('',*,*,#11994,.F.);
#16781=ORIENTED_EDGE('',*,*,#11728,.T.);
#16782=ORIENTED_EDGE('',*,*,#11995,.F.);
#16783=ORIENTED_EDGE('',*,*,#11732,.T.);
#16784=ORIENTED_EDGE('',*,*,#11993,.F.);
#16785=ORIENTED_EDGE('',*,*,#11736,.T.);
#16786=ORIENTED_EDGE('',*,*,#11992,.F.);
#16787=ORIENTED_EDGE('',*,*,#11740,.T.);
#16788=ORIENTED_EDGE('',*,*,#11991,.F.);
#16789=ORIENTED_EDGE('',*,*,#11744,.T.);
#16790=ORIENTED_EDGE('',*,*,#11990,.F.);
#16791=ORIENTED_EDGE('',*,*,#11748,.T.);
#16792=ORIENTED_EDGE('',*,*,#11989,.F.);
#16793=ORIENTED_EDGE('',*,*,#11752,.T.);
#16794=ORIENTED_EDGE('',*,*,#11988,.F.);
#16795=ORIENTED_EDGE('',*,*,#11756,.T.);
#16796=ORIENTED_EDGE('',*,*,#11987,.F.);
#16797=ORIENTED_EDGE('',*,*,#11760,.T.);
#16798=ORIENTED_EDGE('',*,*,#11986,.F.);
#16799=ORIENTED_EDGE('',*,*,#11764,.T.);
#16800=ORIENTED_EDGE('',*,*,#11985,.F.);
#16801=ORIENTED_EDGE('',*,*,#11768,.T.);
#16802=ORIENTED_EDGE('',*,*,#11984,.F.);
#16803=ORIENTED_EDGE('',*,*,#11772,.T.);
#16804=ORIENTED_EDGE('',*,*,#11983,.F.);
#16805=ORIENTED_EDGE('',*,*,#11776,.T.);
#16806=ORIENTED_EDGE('',*,*,#11982,.F.);
#16807=ORIENTED_EDGE('',*,*,#11780,.T.);
#16808=ORIENTED_EDGE('',*,*,#11981,.F.);
#16809=ORIENTED_EDGE('',*,*,#11784,.T.);
#16810=ORIENTED_EDGE('',*,*,#11980,.F.);
#16811=ORIENTED_EDGE('',*,*,#11788,.T.);
#16812=ORIENTED_EDGE('',*,*,#11979,.F.);
#16813=ORIENTED_EDGE('',*,*,#11792,.T.);
#16814=ORIENTED_EDGE('',*,*,#11978,.F.);
#16815=ORIENTED_EDGE('',*,*,#11796,.T.);
#16816=ORIENTED_EDGE('',*,*,#11977,.F.);
#16817=ORIENTED_EDGE('',*,*,#11800,.T.);
#16818=ORIENTED_EDGE('',*,*,#11976,.F.);
#16819=ORIENTED_EDGE('',*,*,#11804,.T.);
#16820=ORIENTED_EDGE('',*,*,#11975,.F.);
#16821=ORIENTED_EDGE('',*,*,#11808,.T.);
#16822=ORIENTED_EDGE('',*,*,#11974,.F.);
#16823=ORIENTED_EDGE('',*,*,#11812,.T.);
#16824=ORIENTED_EDGE('',*,*,#11973,.F.);
#16825=ORIENTED_EDGE('',*,*,#11816,.T.);
#16826=ORIENTED_EDGE('',*,*,#11972,.F.);
#16827=ORIENTED_EDGE('',*,*,#11820,.T.);
#16828=ORIENTED_EDGE('',*,*,#11971,.F.);
#16829=ORIENTED_EDGE('',*,*,#11824,.T.);
#16830=ORIENTED_EDGE('',*,*,#11970,.F.);
#16831=ORIENTED_EDGE('',*,*,#11828,.T.);
#16832=ORIENTED_EDGE('',*,*,#11969,.F.);
#16833=ORIENTED_EDGE('',*,*,#11832,.T.);
#16834=ORIENTED_EDGE('',*,*,#11968,.F.);
#16835=ORIENTED_EDGE('',*,*,#11836,.T.);
#16836=ORIENTED_EDGE('',*,*,#11967,.F.);
#16837=ORIENTED_EDGE('',*,*,#11840,.T.);
#16838=ORIENTED_EDGE('',*,*,#11966,.F.);
#16839=ORIENTED_EDGE('',*,*,#11844,.T.);
#16840=ORIENTED_EDGE('',*,*,#11965,.F.);
#16841=ORIENTED_EDGE('',*,*,#11848,.T.);
#16842=ORIENTED_EDGE('',*,*,#11964,.F.);
#16843=ORIENTED_EDGE('',*,*,#11852,.T.);
#16844=ORIENTED_EDGE('',*,*,#11963,.F.);
#16845=ORIENTED_EDGE('',*,*,#11856,.T.);
#16846=ORIENTED_EDGE('',*,*,#11962,.F.);
#16847=ORIENTED_EDGE('',*,*,#11860,.T.);
#16848=ORIENTED_EDGE('',*,*,#11961,.F.);
#16849=ORIENTED_EDGE('',*,*,#11864,.T.);
#16850=ORIENTED_EDGE('',*,*,#11960,.F.);
#16851=ORIENTED_EDGE('',*,*,#11868,.T.);
#16852=ORIENTED_EDGE('',*,*,#11959,.F.);
#16853=ORIENTED_EDGE('',*,*,#11872,.T.);
#16854=ORIENTED_EDGE('',*,*,#11958,.F.);
#16855=ORIENTED_EDGE('',*,*,#11876,.T.);
#16856=ORIENTED_EDGE('',*,*,#11957,.F.);
#16857=ORIENTED_EDGE('',*,*,#11880,.T.);
#16858=ORIENTED_EDGE('',*,*,#11956,.F.);
#16859=ORIENTED_EDGE('',*,*,#11884,.T.);
#16860=ORIENTED_EDGE('',*,*,#11955,.F.);
#16861=ORIENTED_EDGE('',*,*,#11888,.T.);
#16862=ORIENTED_EDGE('',*,*,#11954,.F.);
#16863=ORIENTED_EDGE('',*,*,#11892,.T.);
#16864=ORIENTED_EDGE('',*,*,#11953,.F.);
#16865=ORIENTED_EDGE('',*,*,#11896,.T.);
#16866=ORIENTED_EDGE('',*,*,#11952,.F.);
#16867=ORIENTED_EDGE('',*,*,#11900,.T.);
#16868=ORIENTED_EDGE('',*,*,#11951,.F.);
#16869=ORIENTED_EDGE('',*,*,#11994,.T.);
#16870=ORIENTED_EDGE('',*,*,#11948,.F.);
#16871=ORIENTED_EDGE('',*,*,#11996,.F.);
#16872=ORIENTED_EDGE('',*,*,#11727,.T.);
#16873=ORIENTED_EDGE('',*,*,#11946,.F.);
#16874=ORIENTED_EDGE('',*,*,#11729,.T.);
#16875=ORIENTED_EDGE('',*,*,#11995,.T.);
#16876=ORIENTED_EDGE('',*,*,#11996,.T.);
#16877=ORIENTED_EDGE('',*,*,#11997,.T.);
#16878=ORIENTED_EDGE('',*,*,#11947,.F.);
#16879=ORIENTED_EDGE('',*,*,#11997,.F.);
#16880=ORIENTED_EDGE('',*,*,#11998,.T.);
#16881=ORIENTED_EDGE('',*,*,#11999,.T.);
#16882=ORIENTED_EDGE('',*,*,#12000,.T.);
#16883=ORIENTED_EDGE('',*,*,#11999,.F.);
#16884=ORIENTED_EDGE('',*,*,#12001,.T.);
#16885=ORIENTED_EDGE('',*,*,#12002,.F.);
#16886=ORIENTED_EDGE('',*,*,#12003,.T.);
#16887=ORIENTED_EDGE('',*,*,#12001,.F.);
#16888=ORIENTED_EDGE('',*,*,#11998,.F.);
#16889=ORIENTED_EDGE('',*,*,#12003,.F.);
#16890=ORIENTED_EDGE('',*,*,#12004,.F.);
#16891=ORIENTED_EDGE('',*,*,#12005,.T.);
#16892=ORIENTED_EDGE('',*,*,#12000,.F.);
#16893=ORIENTED_EDGE('',*,*,#12006,.T.);
#16894=ORIENTED_EDGE('',*,*,#12007,.T.);
#16895=ORIENTED_EDGE('',*,*,#12004,.T.);
#16896=ORIENTED_EDGE('',*,*,#12002,.T.);
#16897=ORIENTED_EDGE('',*,*,#12007,.F.);
#16898=ORIENTED_EDGE('',*,*,#12008,.F.);
#16899=ORIENTED_EDGE('',*,*,#12006,.F.);
#16900=ORIENTED_EDGE('',*,*,#12005,.F.);
#16901=ORIENTED_EDGE('',*,*,#12009,.T.);
#16902=ORIENTED_EDGE('',*,*,#12008,.T.);
#16903=ORIENTED_EDGE('',*,*,#12009,.F.);
#16904=ORIENTED_EDGE('',*,*,#12010,.T.);
#16905=ORIENTED_EDGE('',*,*,#12011,.T.);
#16906=ORIENTED_EDGE('',*,*,#12012,.T.);
#16907=ORIENTED_EDGE('',*,*,#12013,.T.);
#16908=ORIENTED_EDGE('',*,*,#12011,.F.);
#16909=ORIENTED_EDGE('',*,*,#12014,.F.);
#16910=ORIENTED_EDGE('',*,*,#12015,.F.);
#16911=ORIENTED_EDGE('',*,*,#12016,.F.);
#16912=ORIENTED_EDGE('',*,*,#12017,.T.);
#16913=ORIENTED_EDGE('',*,*,#12018,.T.);
#16914=ORIENTED_EDGE('',*,*,#12019,.T.);
#16915=ORIENTED_EDGE('',*,*,#12015,.T.);
#16916=ORIENTED_EDGE('',*,*,#12018,.F.);
#16917=ORIENTED_EDGE('',*,*,#12020,.F.);
#16918=ORIENTED_EDGE('',*,*,#12021,.F.);
#16919=ORIENTED_EDGE('',*,*,#12022,.F.);
#16920=ORIENTED_EDGE('',*,*,#12023,.T.);
#16921=ORIENTED_EDGE('',*,*,#12024,.T.);
#16922=ORIENTED_EDGE('',*,*,#12025,.T.);
#16923=ORIENTED_EDGE('',*,*,#12026,.T.);
#16924=ORIENTED_EDGE('',*,*,#12024,.F.);
#16925=ORIENTED_EDGE('',*,*,#12027,.F.);
#16926=ORIENTED_EDGE('',*,*,#12028,.F.);
#16927=ORIENTED_EDGE('',*,*,#12029,.F.);
#16928=ORIENTED_EDGE('',*,*,#12030,.T.);
#16929=ORIENTED_EDGE('',*,*,#12031,.T.);
#16930=ORIENTED_EDGE('',*,*,#12032,.T.);
#16931=ORIENTED_EDGE('',*,*,#12028,.T.);
#16932=ORIENTED_EDGE('',*,*,#12031,.F.);
#16933=ORIENTED_EDGE('',*,*,#12033,.F.);
#16934=ORIENTED_EDGE('',*,*,#12034,.F.);
#16935=ORIENTED_EDGE('',*,*,#12035,.F.);
#16936=ORIENTED_EDGE('',*,*,#12036,.T.);
#16937=ORIENTED_EDGE('',*,*,#12037,.T.);
#16938=ORIENTED_EDGE('',*,*,#12038,.T.);
#16939=ORIENTED_EDGE('',*,*,#12039,.T.);
#16940=ORIENTED_EDGE('',*,*,#12037,.F.);
#16941=ORIENTED_EDGE('',*,*,#12040,.F.);
#16942=ORIENTED_EDGE('',*,*,#12041,.F.);
#16943=ORIENTED_EDGE('',*,*,#12042,.F.);
#16944=ORIENTED_EDGE('',*,*,#12043,.T.);
#16945=ORIENTED_EDGE('',*,*,#12044,.T.);
#16946=ORIENTED_EDGE('',*,*,#12045,.T.);
#16947=ORIENTED_EDGE('',*,*,#12041,.T.);
#16948=ORIENTED_EDGE('',*,*,#12044,.F.);
#16949=ORIENTED_EDGE('',*,*,#12046,.F.);
#16950=ORIENTED_EDGE('',*,*,#12047,.F.);
#16951=ORIENTED_EDGE('',*,*,#12048,.F.);
#16952=ORIENTED_EDGE('',*,*,#12049,.T.);
#16953=ORIENTED_EDGE('',*,*,#12050,.T.);
#16954=ORIENTED_EDGE('',*,*,#12051,.T.);
#16955=ORIENTED_EDGE('',*,*,#12052,.T.);
#16956=ORIENTED_EDGE('',*,*,#12050,.F.);
#16957=ORIENTED_EDGE('',*,*,#12053,.F.);
#16958=ORIENTED_EDGE('',*,*,#12054,.F.);
#16959=ORIENTED_EDGE('',*,*,#12055,.F.);
#16960=ORIENTED_EDGE('',*,*,#12056,.T.);
#16961=ORIENTED_EDGE('',*,*,#12057,.T.);
#16962=ORIENTED_EDGE('',*,*,#12058,.T.);
#16963=ORIENTED_EDGE('',*,*,#12054,.T.);
#16964=ORIENTED_EDGE('',*,*,#12057,.F.);
#16965=ORIENTED_EDGE('',*,*,#12059,.F.);
#16966=ORIENTED_EDGE('',*,*,#12060,.F.);
#16967=ORIENTED_EDGE('',*,*,#12061,.F.);
#16968=ORIENTED_EDGE('',*,*,#12062,.T.);
#16969=ORIENTED_EDGE('',*,*,#12063,.T.);
#16970=ORIENTED_EDGE('',*,*,#12064,.T.);
#16971=ORIENTED_EDGE('',*,*,#12065,.T.);
#16972=ORIENTED_EDGE('',*,*,#12063,.F.);
#16973=ORIENTED_EDGE('',*,*,#12066,.F.);
#16974=ORIENTED_EDGE('',*,*,#12067,.F.);
#16975=ORIENTED_EDGE('',*,*,#12068,.F.);
#16976=ORIENTED_EDGE('',*,*,#12069,.T.);
#16977=ORIENTED_EDGE('',*,*,#12070,.T.);
#16978=ORIENTED_EDGE('',*,*,#12071,.T.);
#16979=ORIENTED_EDGE('',*,*,#12067,.T.);
#16980=ORIENTED_EDGE('',*,*,#12070,.F.);
#16981=ORIENTED_EDGE('',*,*,#12072,.F.);
#16982=ORIENTED_EDGE('',*,*,#12073,.F.);
#16983=ORIENTED_EDGE('',*,*,#12074,.F.);
#16984=ORIENTED_EDGE('',*,*,#12065,.F.);
#16985=ORIENTED_EDGE('',*,*,#12075,.F.);
#16986=ORIENTED_EDGE('',*,*,#12076,.F.);
#16987=ORIENTED_EDGE('',*,*,#12077,.F.);
#16988=ORIENTED_EDGE('',*,*,#12052,.F.);
#16989=ORIENTED_EDGE('',*,*,#12078,.F.);
#16990=ORIENTED_EDGE('',*,*,#12079,.F.);
#16991=ORIENTED_EDGE('',*,*,#12080,.F.);
#16992=ORIENTED_EDGE('',*,*,#12026,.F.);
#16993=ORIENTED_EDGE('',*,*,#12081,.F.);
#16994=ORIENTED_EDGE('',*,*,#12082,.F.);
#16995=ORIENTED_EDGE('',*,*,#12083,.F.);
#16996=ORIENTED_EDGE('',*,*,#12013,.F.);
#16997=ORIENTED_EDGE('',*,*,#12084,.F.);
#16998=ORIENTED_EDGE('',*,*,#12085,.F.);
#16999=ORIENTED_EDGE('',*,*,#12086,.F.);
#17000=ORIENTED_EDGE('',*,*,#12073,.T.);
#17001=ORIENTED_EDGE('',*,*,#12087,.F.);
#17002=ORIENTED_EDGE('',*,*,#12088,.T.);
#17003=ORIENTED_EDGE('',*,*,#12089,.F.);
#17004=ORIENTED_EDGE('',*,*,#12079,.T.);
#17005=ORIENTED_EDGE('',*,*,#12090,.F.);
#17006=ORIENTED_EDGE('',*,*,#12047,.T.);
#17007=ORIENTED_EDGE('',*,*,#12091,.F.);
#17008=ORIENTED_EDGE('',*,*,#12075,.T.);
#17009=ORIENTED_EDGE('',*,*,#12064,.F.);
#17010=ORIENTED_EDGE('',*,*,#12068,.T.);
#17011=ORIENTED_EDGE('',*,*,#12071,.F.);
#17012=ORIENTED_EDGE('',*,*,#12074,.T.);
#17013=ORIENTED_EDGE('',*,*,#12089,.T.);
#17014=ORIENTED_EDGE('',*,*,#12092,.T.);
#17015=ORIENTED_EDGE('',*,*,#12093,.T.);
#17016=ORIENTED_EDGE('',*,*,#12094,.T.);
#17017=ORIENTED_EDGE('',*,*,#12095,.T.);
#17018=ORIENTED_EDGE('',*,*,#12084,.T.);
#17019=ORIENTED_EDGE('',*,*,#12012,.F.);
#17020=ORIENTED_EDGE('',*,*,#12016,.T.);
#17021=ORIENTED_EDGE('',*,*,#12019,.F.);
#17022=ORIENTED_EDGE('',*,*,#12022,.T.);
#17023=ORIENTED_EDGE('',*,*,#12096,.T.);
#17024=ORIENTED_EDGE('',*,*,#12081,.T.);
#17025=ORIENTED_EDGE('',*,*,#12025,.F.);
#17026=ORIENTED_EDGE('',*,*,#12029,.T.);
#17027=ORIENTED_EDGE('',*,*,#12032,.F.);
#17028=ORIENTED_EDGE('',*,*,#12035,.T.);
#17029=ORIENTED_EDGE('',*,*,#12097,.T.);
#17030=ORIENTED_EDGE('',*,*,#12098,.T.);
#17031=ORIENTED_EDGE('',*,*,#12038,.F.);
#17032=ORIENTED_EDGE('',*,*,#12042,.T.);
#17033=ORIENTED_EDGE('',*,*,#12045,.F.);
#17034=ORIENTED_EDGE('',*,*,#12048,.T.);
#17035=ORIENTED_EDGE('',*,*,#12090,.T.);
#17036=ORIENTED_EDGE('',*,*,#12078,.T.);
#17037=ORIENTED_EDGE('',*,*,#12051,.F.);
#17038=ORIENTED_EDGE('',*,*,#12055,.T.);
#17039=ORIENTED_EDGE('',*,*,#12058,.F.);
#17040=ORIENTED_EDGE('',*,*,#12061,.T.);
#17041=ORIENTED_EDGE('',*,*,#12099,.T.);
#17042=ORIENTED_EDGE('',*,*,#12034,.T.);
#17043=ORIENTED_EDGE('',*,*,#12100,.F.);
#17044=ORIENTED_EDGE('',*,*,#12101,.T.);
#17045=ORIENTED_EDGE('',*,*,#12097,.F.);
#17046=ORIENTED_EDGE('',*,*,#12085,.T.);
#17047=ORIENTED_EDGE('',*,*,#12095,.F.);
#17048=ORIENTED_EDGE('',*,*,#12102,.T.);
#17049=ORIENTED_EDGE('',*,*,#12103,.F.);
#17050=ORIENTED_EDGE('',*,*,#12039,.F.);
#17051=ORIENTED_EDGE('',*,*,#12098,.F.);
#17052=ORIENTED_EDGE('',*,*,#12101,.F.);
#17053=ORIENTED_EDGE('',*,*,#12104,.F.);
#17054=ORIENTED_EDGE('',*,*,#12076,.T.);
#17055=ORIENTED_EDGE('',*,*,#12099,.F.);
#17056=ORIENTED_EDGE('',*,*,#12060,.T.);
#17057=ORIENTED_EDGE('',*,*,#12105,.F.);
#17058=ORIENTED_EDGE('',*,*,#12088,.F.);
#17059=ORIENTED_EDGE('',*,*,#12106,.F.);
#17060=ORIENTED_EDGE('',*,*,#12107,.F.);
#17061=ORIENTED_EDGE('',*,*,#12092,.F.);
#17062=ORIENTED_EDGE('',*,*,#12107,.T.);
#17063=ORIENTED_EDGE('',*,*,#12108,.F.);
#17064=ORIENTED_EDGE('',*,*,#12109,.F.);
#17065=ORIENTED_EDGE('',*,*,#12093,.F.);
#17066=ORIENTED_EDGE('',*,*,#12109,.T.);
#17067=ORIENTED_EDGE('',*,*,#12110,.F.);
#17068=ORIENTED_EDGE('',*,*,#12102,.F.);
#17069=ORIENTED_EDGE('',*,*,#12094,.F.);
#17070=ORIENTED_EDGE('',*,*,#12082,.T.);
#17071=ORIENTED_EDGE('',*,*,#12096,.F.);
#17072=ORIENTED_EDGE('',*,*,#12021,.T.);
#17073=ORIENTED_EDGE('',*,*,#12111,.F.);
#17074=ORIENTED_EDGE('',*,*,#12077,.T.);
#17075=ORIENTED_EDGE('',*,*,#12105,.T.);
#17076=ORIENTED_EDGE('',*,*,#12059,.T.);
#17077=ORIENTED_EDGE('',*,*,#12056,.F.);
#17078=ORIENTED_EDGE('',*,*,#12053,.T.);
#17079=ORIENTED_EDGE('',*,*,#12049,.F.);
#17080=ORIENTED_EDGE('',*,*,#12080,.T.);
#17081=ORIENTED_EDGE('',*,*,#12091,.T.);
#17082=ORIENTED_EDGE('',*,*,#12046,.T.);
#17083=ORIENTED_EDGE('',*,*,#12043,.F.);
#17084=ORIENTED_EDGE('',*,*,#12040,.T.);
#17085=ORIENTED_EDGE('',*,*,#12036,.F.);
#17086=ORIENTED_EDGE('',*,*,#12104,.T.);
#17087=ORIENTED_EDGE('',*,*,#12100,.T.);
#17088=ORIENTED_EDGE('',*,*,#12033,.T.);
#17089=ORIENTED_EDGE('',*,*,#12030,.F.);
#17090=ORIENTED_EDGE('',*,*,#12027,.T.);
#17091=ORIENTED_EDGE('',*,*,#12023,.F.);
#17092=ORIENTED_EDGE('',*,*,#12083,.T.);
#17093=ORIENTED_EDGE('',*,*,#12111,.T.);
#17094=ORIENTED_EDGE('',*,*,#12020,.T.);
#17095=ORIENTED_EDGE('',*,*,#12017,.F.);
#17096=ORIENTED_EDGE('',*,*,#12014,.T.);
#17097=ORIENTED_EDGE('',*,*,#12010,.F.);
#17098=ORIENTED_EDGE('',*,*,#12086,.T.);
#17099=ORIENTED_EDGE('',*,*,#12103,.T.);
#17100=ORIENTED_EDGE('',*,*,#12110,.T.);
#17101=ORIENTED_EDGE('',*,*,#12108,.T.);
#17102=ORIENTED_EDGE('',*,*,#12106,.T.);
#17103=ORIENTED_EDGE('',*,*,#12087,.T.);
#17104=ORIENTED_EDGE('',*,*,#12072,.T.);
#17105=ORIENTED_EDGE('',*,*,#12069,.F.);
#17106=ORIENTED_EDGE('',*,*,#12066,.T.);
#17107=ORIENTED_EDGE('',*,*,#12062,.F.);
#17108=ORIENTED_EDGE('',*,*,#12112,.T.);
#17109=ORIENTED_EDGE('',*,*,#12113,.T.);
#17110=ORIENTED_EDGE('',*,*,#12114,.T.);
#17111=ORIENTED_EDGE('',*,*,#12115,.F.);
#17112=ORIENTED_EDGE('',*,*,#12116,.F.);
#17113=ORIENTED_EDGE('',*,*,#12117,.T.);
#17114=ORIENTED_EDGE('',*,*,#12118,.T.);
#17115=ORIENTED_EDGE('',*,*,#12119,.F.);
#17116=ORIENTED_EDGE('',*,*,#12114,.F.);
#17117=ORIENTED_EDGE('',*,*,#12120,.F.);
#17118=ORIENTED_EDGE('',*,*,#12118,.F.);
#17119=ORIENTED_EDGE('',*,*,#12121,.F.);
#17120=ORIENTED_EDGE('',*,*,#12122,.T.);
#17121=ORIENTED_EDGE('',*,*,#12119,.T.);
#17122=ORIENTED_EDGE('',*,*,#12120,.T.);
#17123=ORIENTED_EDGE('',*,*,#12113,.F.);
#17124=ORIENTED_EDGE('',*,*,#12123,.T.);
#17125=ORIENTED_EDGE('',*,*,#12124,.F.);
#17126=ORIENTED_EDGE('',*,*,#12125,.F.);
#17127=ORIENTED_EDGE('',*,*,#12126,.F.);
#17128=ORIENTED_EDGE('',*,*,#12127,.T.);
#17129=ORIENTED_EDGE('',*,*,#12116,.T.);
#17130=ORIENTED_EDGE('',*,*,#12122,.F.);
#17131=ORIENTED_EDGE('',*,*,#12115,.T.);
#17132=ORIENTED_EDGE('',*,*,#12121,.T.);
#17133=ORIENTED_EDGE('',*,*,#12117,.F.);
#17134=ORIENTED_EDGE('',*,*,#12127,.F.);
#17135=ORIENTED_EDGE('',*,*,#12128,.F.);
#17136=ORIENTED_EDGE('',*,*,#12129,.F.);
#17137=ORIENTED_EDGE('',*,*,#12130,.F.);
#17138=ORIENTED_EDGE('',*,*,#12130,.T.);
#17139=ORIENTED_EDGE('',*,*,#12131,.F.);
#17140=ORIENTED_EDGE('',*,*,#12123,.F.);
#17141=ORIENTED_EDGE('',*,*,#12112,.F.);
#17142=ORIENTED_EDGE('',*,*,#12125,.T.);
#17143=ORIENTED_EDGE('',*,*,#12132,.F.);
#17144=ORIENTED_EDGE('',*,*,#12128,.T.);
#17145=ORIENTED_EDGE('',*,*,#12126,.T.);
#17146=ORIENTED_EDGE('',*,*,#12132,.T.);
#17147=ORIENTED_EDGE('',*,*,#12124,.T.);
#17148=ORIENTED_EDGE('',*,*,#12131,.T.);
#17149=ORIENTED_EDGE('',*,*,#12129,.T.);
#17150=ORIENTED_EDGE('',*,*,#12133,.T.);
#17151=ORIENTED_EDGE('',*,*,#12134,.T.);
#17152=ORIENTED_EDGE('',*,*,#12135,.F.);
#17153=ORIENTED_EDGE('',*,*,#12136,.T.);
#17154=ORIENTED_EDGE('',*,*,#12137,.T.);
#17155=ORIENTED_EDGE('',*,*,#12138,.F.);
#17156=ORIENTED_EDGE('',*,*,#12133,.F.);
#17157=ORIENTED_EDGE('',*,*,#12139,.F.);
#17158=ORIENTED_EDGE('',*,*,#12140,.T.);
#17159=ORIENTED_EDGE('',*,*,#12141,.T.);
#17160=ORIENTED_EDGE('',*,*,#12137,.F.);
#17161=ORIENTED_EDGE('',*,*,#12142,.T.);
#17162=ORIENTED_EDGE('',*,*,#12143,.T.);
#17163=ORIENTED_EDGE('',*,*,#12144,.F.);
#17164=ORIENTED_EDGE('',*,*,#12140,.F.);
#17165=ORIENTED_EDGE('',*,*,#12145,.F.);
#17166=ORIENTED_EDGE('',*,*,#12146,.T.);
#17167=ORIENTED_EDGE('',*,*,#12147,.T.);
#17168=ORIENTED_EDGE('',*,*,#12143,.F.);
#17169=ORIENTED_EDGE('',*,*,#12148,.T.);
#17170=ORIENTED_EDGE('',*,*,#12149,.T.);
#17171=ORIENTED_EDGE('',*,*,#12150,.F.);
#17172=ORIENTED_EDGE('',*,*,#12146,.F.);
#17173=ORIENTED_EDGE('',*,*,#12151,.F.);
#17174=ORIENTED_EDGE('',*,*,#12152,.T.);
#17175=ORIENTED_EDGE('',*,*,#12153,.T.);
#17176=ORIENTED_EDGE('',*,*,#12149,.F.);
#17177=ORIENTED_EDGE('',*,*,#12154,.T.);
#17178=ORIENTED_EDGE('',*,*,#12155,.F.);
#17179=ORIENTED_EDGE('',*,*,#12156,.F.);
#17180=ORIENTED_EDGE('',*,*,#12152,.F.);
#17181=ORIENTED_EDGE('',*,*,#12157,.F.);
#17182=ORIENTED_EDGE('',*,*,#12158,.T.);
#17183=ORIENTED_EDGE('',*,*,#12159,.T.);
#17184=ORIENTED_EDGE('',*,*,#12160,.F.);
#17185=ORIENTED_EDGE('',*,*,#12161,.T.);
#17186=ORIENTED_EDGE('',*,*,#12160,.T.);
#17187=ORIENTED_EDGE('',*,*,#12162,.F.);
#17188=ORIENTED_EDGE('',*,*,#12163,.F.);
#17189=ORIENTED_EDGE('',*,*,#12164,.F.);
#17190=ORIENTED_EDGE('',*,*,#12163,.T.);
#17191=ORIENTED_EDGE('',*,*,#12165,.T.);
#17192=ORIENTED_EDGE('',*,*,#12166,.F.);
#17193=ORIENTED_EDGE('',*,*,#12167,.T.);
#17194=ORIENTED_EDGE('',*,*,#12166,.T.);
#17195=ORIENTED_EDGE('',*,*,#12168,.F.);
#17196=ORIENTED_EDGE('',*,*,#12169,.F.);
#17197=ORIENTED_EDGE('',*,*,#12170,.F.);
#17198=ORIENTED_EDGE('',*,*,#12169,.T.);
#17199=ORIENTED_EDGE('',*,*,#12171,.T.);
#17200=ORIENTED_EDGE('',*,*,#12172,.F.);
#17201=ORIENTED_EDGE('',*,*,#12173,.T.);
#17202=ORIENTED_EDGE('',*,*,#12172,.T.);
#17203=ORIENTED_EDGE('',*,*,#12174,.F.);
#17204=ORIENTED_EDGE('',*,*,#12175,.F.);
#17205=ORIENTED_EDGE('',*,*,#12176,.F.);
#17206=ORIENTED_EDGE('',*,*,#12175,.T.);
#17207=ORIENTED_EDGE('',*,*,#12177,.T.);
#17208=ORIENTED_EDGE('',*,*,#12155,.T.);
#17209=ORIENTED_EDGE('',*,*,#12178,.T.);
#17210=ORIENTED_EDGE('',*,*,#12159,.F.);
#17211=ORIENTED_EDGE('',*,*,#12179,.T.);
#17212=ORIENTED_EDGE('',*,*,#12134,.F.);
#17213=ORIENTED_EDGE('',*,*,#12138,.T.);
#17214=ORIENTED_EDGE('',*,*,#12141,.F.);
#17215=ORIENTED_EDGE('',*,*,#12144,.T.);
#17216=ORIENTED_EDGE('',*,*,#12147,.F.);
#17217=ORIENTED_EDGE('',*,*,#12150,.T.);
#17218=ORIENTED_EDGE('',*,*,#12153,.F.);
#17219=ORIENTED_EDGE('',*,*,#12156,.T.);
#17220=ORIENTED_EDGE('',*,*,#12177,.F.);
#17221=ORIENTED_EDGE('',*,*,#12174,.T.);
#17222=ORIENTED_EDGE('',*,*,#12171,.F.);
#17223=ORIENTED_EDGE('',*,*,#12168,.T.);
#17224=ORIENTED_EDGE('',*,*,#12165,.F.);
#17225=ORIENTED_EDGE('',*,*,#12162,.T.);
#17226=ORIENTED_EDGE('',*,*,#12180,.T.);
#17227=ORIENTED_EDGE('',*,*,#12181,.T.);
#17228=ORIENTED_EDGE('',*,*,#12182,.T.);
#17229=ORIENTED_EDGE('',*,*,#12183,.T.);
#17230=ORIENTED_EDGE('',*,*,#12184,.T.);
#17231=ORIENTED_EDGE('',*,*,#12185,.T.);
#17232=ORIENTED_EDGE('',*,*,#12186,.T.);
#17233=ORIENTED_EDGE('',*,*,#12187,.T.);
#17234=ORIENTED_EDGE('',*,*,#12188,.T.);
#17235=ORIENTED_EDGE('',*,*,#12189,.T.);
#17236=ORIENTED_EDGE('',*,*,#12190,.T.);
#17237=ORIENTED_EDGE('',*,*,#12191,.T.);
#17238=ORIENTED_EDGE('',*,*,#12135,.T.);
#17239=ORIENTED_EDGE('',*,*,#12179,.F.);
#17240=ORIENTED_EDGE('',*,*,#12158,.F.);
#17241=ORIENTED_EDGE('',*,*,#12192,.F.);
#17242=ORIENTED_EDGE('',*,*,#12180,.F.);
#17243=ORIENTED_EDGE('',*,*,#12193,.T.);
#17244=ORIENTED_EDGE('',*,*,#12194,.F.);
#17245=ORIENTED_EDGE('',*,*,#12193,.F.);
#17246=ORIENTED_EDGE('',*,*,#12181,.F.);
#17247=ORIENTED_EDGE('',*,*,#12195,.T.);
#17248=ORIENTED_EDGE('',*,*,#12196,.F.);
#17249=ORIENTED_EDGE('',*,*,#12195,.F.);
#17250=ORIENTED_EDGE('',*,*,#12182,.F.);
#17251=ORIENTED_EDGE('',*,*,#12197,.T.);
#17252=ORIENTED_EDGE('',*,*,#12198,.F.);
#17253=ORIENTED_EDGE('',*,*,#12197,.F.);
#17254=ORIENTED_EDGE('',*,*,#12183,.F.);
#17255=ORIENTED_EDGE('',*,*,#12199,.T.);
#17256=ORIENTED_EDGE('',*,*,#12200,.F.);
#17257=ORIENTED_EDGE('',*,*,#12199,.F.);
#17258=ORIENTED_EDGE('',*,*,#12201,.F.);
#17259=ORIENTED_EDGE('',*,*,#12202,.F.);
#17260=ORIENTED_EDGE('',*,*,#12203,.F.);
#17261=ORIENTED_EDGE('',*,*,#12185,.F.);
#17262=ORIENTED_EDGE('',*,*,#12203,.T.);
#17263=ORIENTED_EDGE('',*,*,#12204,.F.);
#17264=ORIENTED_EDGE('',*,*,#12205,.F.);
#17265=ORIENTED_EDGE('',*,*,#12186,.F.);
#17266=ORIENTED_EDGE('',*,*,#12205,.T.);
#17267=ORIENTED_EDGE('',*,*,#12206,.F.);
#17268=ORIENTED_EDGE('',*,*,#12207,.F.);
#17269=ORIENTED_EDGE('',*,*,#12187,.F.);
#17270=ORIENTED_EDGE('',*,*,#12207,.T.);
#17271=ORIENTED_EDGE('',*,*,#12208,.F.);
#17272=ORIENTED_EDGE('',*,*,#12209,.F.);
#17273=ORIENTED_EDGE('',*,*,#12188,.F.);
#17274=ORIENTED_EDGE('',*,*,#12209,.T.);
#17275=ORIENTED_EDGE('',*,*,#12210,.F.);
#17276=ORIENTED_EDGE('',*,*,#12211,.F.);
#17277=ORIENTED_EDGE('',*,*,#12189,.F.);
#17278=ORIENTED_EDGE('',*,*,#12211,.T.);
#17279=ORIENTED_EDGE('',*,*,#12212,.F.);
#17280=ORIENTED_EDGE('',*,*,#12213,.F.);
#17281=ORIENTED_EDGE('',*,*,#12190,.F.);
#17282=ORIENTED_EDGE('',*,*,#12213,.T.);
#17283=ORIENTED_EDGE('',*,*,#12214,.F.);
#17284=ORIENTED_EDGE('',*,*,#12215,.F.);
#17285=ORIENTED_EDGE('',*,*,#12191,.F.);
#17286=ORIENTED_EDGE('',*,*,#12215,.T.);
#17287=ORIENTED_EDGE('',*,*,#12216,.F.);
#17288=ORIENTED_EDGE('',*,*,#12201,.T.);
#17289=ORIENTED_EDGE('',*,*,#12184,.F.);
#17290=ORIENTED_EDGE('',*,*,#12161,.F.);
#17291=ORIENTED_EDGE('',*,*,#12164,.T.);
#17292=ORIENTED_EDGE('',*,*,#12167,.F.);
#17293=ORIENTED_EDGE('',*,*,#12170,.T.);
#17294=ORIENTED_EDGE('',*,*,#12173,.F.);
#17295=ORIENTED_EDGE('',*,*,#12176,.T.);
#17296=ORIENTED_EDGE('',*,*,#12178,.F.);
#17297=ORIENTED_EDGE('',*,*,#12157,.T.);
#17298=ORIENTED_EDGE('',*,*,#12154,.F.);
#17299=ORIENTED_EDGE('',*,*,#12151,.T.);
#17300=ORIENTED_EDGE('',*,*,#12148,.F.);
#17301=ORIENTED_EDGE('',*,*,#12145,.T.);
#17302=ORIENTED_EDGE('',*,*,#12142,.F.);
#17303=ORIENTED_EDGE('',*,*,#12139,.T.);
#17304=ORIENTED_EDGE('',*,*,#12136,.F.);
#17305=ORIENTED_EDGE('',*,*,#12192,.T.);
#17306=ORIENTED_EDGE('',*,*,#12194,.T.);
#17307=ORIENTED_EDGE('',*,*,#12196,.T.);
#17308=ORIENTED_EDGE('',*,*,#12198,.T.);
#17309=ORIENTED_EDGE('',*,*,#12200,.T.);
#17310=ORIENTED_EDGE('',*,*,#12216,.T.);
#17311=ORIENTED_EDGE('',*,*,#12214,.T.);
#17312=ORIENTED_EDGE('',*,*,#12212,.T.);
#17313=ORIENTED_EDGE('',*,*,#12210,.T.);
#17314=ORIENTED_EDGE('',*,*,#12208,.T.);
#17315=ORIENTED_EDGE('',*,*,#12206,.T.);
#17316=ORIENTED_EDGE('',*,*,#12204,.T.);
#17317=ORIENTED_EDGE('',*,*,#12202,.T.);
#17318=ORIENTED_EDGE('',*,*,#12217,.T.);
#17319=ORIENTED_EDGE('',*,*,#12218,.T.);
#17320=ORIENTED_EDGE('',*,*,#12219,.T.);
#17321=ORIENTED_EDGE('',*,*,#12220,.T.);
#17322=ORIENTED_EDGE('',*,*,#12218,.F.);
#17323=ORIENTED_EDGE('',*,*,#12221,.F.);
#17324=ORIENTED_EDGE('',*,*,#12222,.F.);
#17325=ORIENTED_EDGE('',*,*,#12223,.F.);
#17326=ORIENTED_EDGE('',*,*,#12224,.T.);
#17327=ORIENTED_EDGE('',*,*,#12225,.T.);
#17328=ORIENTED_EDGE('',*,*,#12226,.T.);
#17329=ORIENTED_EDGE('',*,*,#12222,.T.);
#17330=ORIENTED_EDGE('',*,*,#12225,.F.);
#17331=ORIENTED_EDGE('',*,*,#12227,.F.);
#17332=ORIENTED_EDGE('',*,*,#12228,.F.);
#17333=ORIENTED_EDGE('',*,*,#12229,.F.);
#17334=ORIENTED_EDGE('',*,*,#12230,.T.);
#17335=ORIENTED_EDGE('',*,*,#12231,.T.);
#17336=ORIENTED_EDGE('',*,*,#12232,.T.);
#17337=ORIENTED_EDGE('',*,*,#12233,.T.);
#17338=ORIENTED_EDGE('',*,*,#12231,.F.);
#17339=ORIENTED_EDGE('',*,*,#12234,.F.);
#17340=ORIENTED_EDGE('',*,*,#12235,.F.);
#17341=ORIENTED_EDGE('',*,*,#12236,.F.);
#17342=ORIENTED_EDGE('',*,*,#12237,.T.);
#17343=ORIENTED_EDGE('',*,*,#12238,.T.);
#17344=ORIENTED_EDGE('',*,*,#12239,.T.);
#17345=ORIENTED_EDGE('',*,*,#12235,.T.);
#17346=ORIENTED_EDGE('',*,*,#12238,.F.);
#17347=ORIENTED_EDGE('',*,*,#12240,.F.);
#17348=ORIENTED_EDGE('',*,*,#12241,.F.);
#17349=ORIENTED_EDGE('',*,*,#12242,.F.);
#17350=ORIENTED_EDGE('',*,*,#12243,.T.);
#17351=ORIENTED_EDGE('',*,*,#12244,.T.);
#17352=ORIENTED_EDGE('',*,*,#12245,.T.);
#17353=ORIENTED_EDGE('',*,*,#12246,.T.);
#17354=ORIENTED_EDGE('',*,*,#12244,.F.);
#17355=ORIENTED_EDGE('',*,*,#12247,.F.);
#17356=ORIENTED_EDGE('',*,*,#12248,.F.);
#17357=ORIENTED_EDGE('',*,*,#12249,.F.);
#17358=ORIENTED_EDGE('',*,*,#12250,.T.);
#17359=ORIENTED_EDGE('',*,*,#12251,.T.);
#17360=ORIENTED_EDGE('',*,*,#12252,.T.);
#17361=ORIENTED_EDGE('',*,*,#12248,.T.);
#17362=ORIENTED_EDGE('',*,*,#12251,.F.);
#17363=ORIENTED_EDGE('',*,*,#12253,.F.);
#17364=ORIENTED_EDGE('',*,*,#12254,.F.);
#17365=ORIENTED_EDGE('',*,*,#12255,.F.);
#17366=ORIENTED_EDGE('',*,*,#12256,.T.);
#17367=ORIENTED_EDGE('',*,*,#12257,.T.);
#17368=ORIENTED_EDGE('',*,*,#12258,.T.);
#17369=ORIENTED_EDGE('',*,*,#12259,.T.);
#17370=ORIENTED_EDGE('',*,*,#12257,.F.);
#17371=ORIENTED_EDGE('',*,*,#12260,.F.);
#17372=ORIENTED_EDGE('',*,*,#12261,.F.);
#17373=ORIENTED_EDGE('',*,*,#12262,.F.);
#17374=ORIENTED_EDGE('',*,*,#12263,.T.);
#17375=ORIENTED_EDGE('',*,*,#12264,.T.);
#17376=ORIENTED_EDGE('',*,*,#12265,.T.);
#17377=ORIENTED_EDGE('',*,*,#12261,.T.);
#17378=ORIENTED_EDGE('',*,*,#12264,.F.);
#17379=ORIENTED_EDGE('',*,*,#12266,.F.);
#17380=ORIENTED_EDGE('',*,*,#12267,.F.);
#17381=ORIENTED_EDGE('',*,*,#12268,.F.);
#17382=ORIENTED_EDGE('',*,*,#12269,.T.);
#17383=ORIENTED_EDGE('',*,*,#12270,.T.);
#17384=ORIENTED_EDGE('',*,*,#12271,.T.);
#17385=ORIENTED_EDGE('',*,*,#12272,.T.);
#17386=ORIENTED_EDGE('',*,*,#12270,.F.);
#17387=ORIENTED_EDGE('',*,*,#12273,.F.);
#17388=ORIENTED_EDGE('',*,*,#12274,.F.);
#17389=ORIENTED_EDGE('',*,*,#12275,.F.);
#17390=ORIENTED_EDGE('',*,*,#12276,.T.);
#17391=ORIENTED_EDGE('',*,*,#12277,.T.);
#17392=ORIENTED_EDGE('',*,*,#12278,.T.);
#17393=ORIENTED_EDGE('',*,*,#12274,.T.);
#17394=ORIENTED_EDGE('',*,*,#12277,.F.);
#17395=ORIENTED_EDGE('',*,*,#12279,.F.);
#17396=ORIENTED_EDGE('',*,*,#12280,.F.);
#17397=ORIENTED_EDGE('',*,*,#12281,.F.);
#17398=ORIENTED_EDGE('',*,*,#12272,.F.);
#17399=ORIENTED_EDGE('',*,*,#12282,.F.);
#17400=ORIENTED_EDGE('',*,*,#12283,.F.);
#17401=ORIENTED_EDGE('',*,*,#12284,.F.);
#17402=ORIENTED_EDGE('',*,*,#12259,.F.);
#17403=ORIENTED_EDGE('',*,*,#12285,.F.);
#17404=ORIENTED_EDGE('',*,*,#12286,.F.);
#17405=ORIENTED_EDGE('',*,*,#12287,.F.);
#17406=ORIENTED_EDGE('',*,*,#12233,.F.);
#17407=ORIENTED_EDGE('',*,*,#12288,.F.);
#17408=ORIENTED_EDGE('',*,*,#12289,.F.);
#17409=ORIENTED_EDGE('',*,*,#12290,.F.);
#17410=ORIENTED_EDGE('',*,*,#12220,.F.);
#17411=ORIENTED_EDGE('',*,*,#12291,.F.);
#17412=ORIENTED_EDGE('',*,*,#12292,.F.);
#17413=ORIENTED_EDGE('',*,*,#12293,.F.);
#17414=ORIENTED_EDGE('',*,*,#12280,.T.);
#17415=ORIENTED_EDGE('',*,*,#12294,.F.);
#17416=ORIENTED_EDGE('',*,*,#12295,.F.);
#17417=ORIENTED_EDGE('',*,*,#12296,.F.);
#17418=ORIENTED_EDGE('',*,*,#12286,.T.);
#17419=ORIENTED_EDGE('',*,*,#12297,.F.);
#17420=ORIENTED_EDGE('',*,*,#12254,.T.);
#17421=ORIENTED_EDGE('',*,*,#12298,.F.);
#17422=ORIENTED_EDGE('',*,*,#12282,.T.);
#17423=ORIENTED_EDGE('',*,*,#12271,.F.);
#17424=ORIENTED_EDGE('',*,*,#12275,.T.);
#17425=ORIENTED_EDGE('',*,*,#12278,.F.);
#17426=ORIENTED_EDGE('',*,*,#12281,.T.);
#17427=ORIENTED_EDGE('',*,*,#12296,.T.);
#17428=ORIENTED_EDGE('',*,*,#12299,.T.);
#17429=ORIENTED_EDGE('',*,*,#12300,.T.);
#17430=ORIENTED_EDGE('',*,*,#12301,.T.);
#17431=ORIENTED_EDGE('',*,*,#12302,.T.);
#17432=ORIENTED_EDGE('',*,*,#12291,.T.);
#17433=ORIENTED_EDGE('',*,*,#12219,.F.);
#17434=ORIENTED_EDGE('',*,*,#12223,.T.);
#17435=ORIENTED_EDGE('',*,*,#12226,.F.);
#17436=ORIENTED_EDGE('',*,*,#12229,.T.);
#17437=ORIENTED_EDGE('',*,*,#12303,.T.);
#17438=ORIENTED_EDGE('',*,*,#12288,.T.);
#17439=ORIENTED_EDGE('',*,*,#12232,.F.);
#17440=ORIENTED_EDGE('',*,*,#12236,.T.);
#17441=ORIENTED_EDGE('',*,*,#12239,.F.);
#17442=ORIENTED_EDGE('',*,*,#12242,.T.);
#17443=ORIENTED_EDGE('',*,*,#12304,.T.);
#17444=ORIENTED_EDGE('',*,*,#12305,.T.);
#17445=ORIENTED_EDGE('',*,*,#12245,.F.);
#17446=ORIENTED_EDGE('',*,*,#12249,.T.);
#17447=ORIENTED_EDGE('',*,*,#12252,.F.);
#17448=ORIENTED_EDGE('',*,*,#12255,.T.);
#17449=ORIENTED_EDGE('',*,*,#12297,.T.);
#17450=ORIENTED_EDGE('',*,*,#12285,.T.);
#17451=ORIENTED_EDGE('',*,*,#12258,.F.);
#17452=ORIENTED_EDGE('',*,*,#12262,.T.);
#17453=ORIENTED_EDGE('',*,*,#12265,.F.);
#17454=ORIENTED_EDGE('',*,*,#12268,.T.);
#17455=ORIENTED_EDGE('',*,*,#12306,.T.);
#17456=ORIENTED_EDGE('',*,*,#12241,.T.);
#17457=ORIENTED_EDGE('',*,*,#12307,.F.);
#17458=ORIENTED_EDGE('',*,*,#12308,.T.);
#17459=ORIENTED_EDGE('',*,*,#12304,.F.);
#17460=ORIENTED_EDGE('',*,*,#12292,.T.);
#17461=ORIENTED_EDGE('',*,*,#12302,.F.);
#17462=ORIENTED_EDGE('',*,*,#12309,.T.);
#17463=ORIENTED_EDGE('',*,*,#12310,.F.);
#17464=ORIENTED_EDGE('',*,*,#12246,.F.);
#17465=ORIENTED_EDGE('',*,*,#12305,.F.);
#17466=ORIENTED_EDGE('',*,*,#12308,.F.);
#17467=ORIENTED_EDGE('',*,*,#12311,.F.);
#17468=ORIENTED_EDGE('',*,*,#12283,.T.);
#17469=ORIENTED_EDGE('',*,*,#12306,.F.);
#17470=ORIENTED_EDGE('',*,*,#12267,.T.);
#17471=ORIENTED_EDGE('',*,*,#12312,.F.);
#17472=ORIENTED_EDGE('',*,*,#12313,.F.);
#17473=ORIENTED_EDGE('',*,*,#12314,.F.);
#17474=ORIENTED_EDGE('',*,*,#12315,.F.);
#17475=ORIENTED_EDGE('',*,*,#12300,.F.);
#17476=ORIENTED_EDGE('',*,*,#12315,.T.);
#17477=ORIENTED_EDGE('',*,*,#12316,.F.);
#17478=ORIENTED_EDGE('',*,*,#12309,.F.);
#17479=ORIENTED_EDGE('',*,*,#12301,.F.);
#17480=ORIENTED_EDGE('',*,*,#12289,.T.);
#17481=ORIENTED_EDGE('',*,*,#12303,.F.);
#17482=ORIENTED_EDGE('',*,*,#12228,.T.);
#17483=ORIENTED_EDGE('',*,*,#12317,.F.);
#17484=ORIENTED_EDGE('',*,*,#12295,.T.);
#17485=ORIENTED_EDGE('',*,*,#12318,.F.);
#17486=ORIENTED_EDGE('',*,*,#12313,.T.);
#17487=ORIENTED_EDGE('',*,*,#12299,.F.);
#17488=ORIENTED_EDGE('',*,*,#12284,.T.);
#17489=ORIENTED_EDGE('',*,*,#12312,.T.);
#17490=ORIENTED_EDGE('',*,*,#12266,.T.);
#17491=ORIENTED_EDGE('',*,*,#12263,.F.);
#17492=ORIENTED_EDGE('',*,*,#12260,.T.);
#17493=ORIENTED_EDGE('',*,*,#12256,.F.);
#17494=ORIENTED_EDGE('',*,*,#12287,.T.);
#17495=ORIENTED_EDGE('',*,*,#12298,.T.);
#17496=ORIENTED_EDGE('',*,*,#12253,.T.);
#17497=ORIENTED_EDGE('',*,*,#12250,.F.);
#17498=ORIENTED_EDGE('',*,*,#12247,.T.);
#17499=ORIENTED_EDGE('',*,*,#12243,.F.);
#17500=ORIENTED_EDGE('',*,*,#12311,.T.);
#17501=ORIENTED_EDGE('',*,*,#12307,.T.);
#17502=ORIENTED_EDGE('',*,*,#12240,.T.);
#17503=ORIENTED_EDGE('',*,*,#12237,.F.);
#17504=ORIENTED_EDGE('',*,*,#12234,.T.);
#17505=ORIENTED_EDGE('',*,*,#12230,.F.);
#17506=ORIENTED_EDGE('',*,*,#12290,.T.);
#17507=ORIENTED_EDGE('',*,*,#12317,.T.);
#17508=ORIENTED_EDGE('',*,*,#12227,.T.);
#17509=ORIENTED_EDGE('',*,*,#12224,.F.);
#17510=ORIENTED_EDGE('',*,*,#12221,.T.);
#17511=ORIENTED_EDGE('',*,*,#12217,.F.);
#17512=ORIENTED_EDGE('',*,*,#12293,.T.);
#17513=ORIENTED_EDGE('',*,*,#12310,.T.);
#17514=ORIENTED_EDGE('',*,*,#12316,.T.);
#17515=ORIENTED_EDGE('',*,*,#12314,.T.);
#17516=ORIENTED_EDGE('',*,*,#12318,.T.);
#17517=ORIENTED_EDGE('',*,*,#12294,.T.);
#17518=ORIENTED_EDGE('',*,*,#12279,.T.);
#17519=ORIENTED_EDGE('',*,*,#12276,.F.);
#17520=ORIENTED_EDGE('',*,*,#12273,.T.);
#17521=ORIENTED_EDGE('',*,*,#12269,.F.);
#17522=ORIENTED_EDGE('',*,*,#12319,.F.);
#17523=ORIENTED_EDGE('',*,*,#12320,.F.);
#17524=ORIENTED_EDGE('',*,*,#12321,.F.);
#17525=ORIENTED_EDGE('',*,*,#12322,.T.);
#17526=ORIENTED_EDGE('',*,*,#12323,.F.);
#17527=ORIENTED_EDGE('',*,*,#12322,.F.);
#17528=ORIENTED_EDGE('',*,*,#12324,.F.);
#17529=ORIENTED_EDGE('',*,*,#12325,.T.);
#17530=ORIENTED_EDGE('',*,*,#12326,.F.);
#17531=ORIENTED_EDGE('',*,*,#12325,.F.);
#17532=ORIENTED_EDGE('',*,*,#12327,.F.);
#17533=ORIENTED_EDGE('',*,*,#12328,.T.);
#17534=ORIENTED_EDGE('',*,*,#12329,.F.);
#17535=ORIENTED_EDGE('',*,*,#12328,.F.);
#17536=ORIENTED_EDGE('',*,*,#12330,.F.);
#17537=ORIENTED_EDGE('',*,*,#12320,.T.);
#17538=ORIENTED_EDGE('',*,*,#12331,.F.);
#17539=ORIENTED_EDGE('',*,*,#12332,.F.);
#17540=ORIENTED_EDGE('',*,*,#12333,.F.);
#17541=ORIENTED_EDGE('',*,*,#12334,.T.);
#17542=ORIENTED_EDGE('',*,*,#12335,.F.);
#17543=ORIENTED_EDGE('',*,*,#12334,.F.);
#17544=ORIENTED_EDGE('',*,*,#12336,.F.);
#17545=ORIENTED_EDGE('',*,*,#12337,.T.);
#17546=ORIENTED_EDGE('',*,*,#12338,.F.);
#17547=ORIENTED_EDGE('',*,*,#12337,.F.);
#17548=ORIENTED_EDGE('',*,*,#12339,.F.);
#17549=ORIENTED_EDGE('',*,*,#12340,.T.);
#17550=ORIENTED_EDGE('',*,*,#12341,.F.);
#17551=ORIENTED_EDGE('',*,*,#12340,.F.);
#17552=ORIENTED_EDGE('',*,*,#12342,.F.);
#17553=ORIENTED_EDGE('',*,*,#12332,.T.);
#17554=ORIENTED_EDGE('',*,*,#12343,.F.);
#17555=ORIENTED_EDGE('',*,*,#12344,.F.);
#17556=ORIENTED_EDGE('',*,*,#12345,.F.);
#17557=ORIENTED_EDGE('',*,*,#12346,.T.);
#17558=ORIENTED_EDGE('',*,*,#12347,.F.);
#17559=ORIENTED_EDGE('',*,*,#12346,.F.);
#17560=ORIENTED_EDGE('',*,*,#12348,.F.);
#17561=ORIENTED_EDGE('',*,*,#12349,.T.);
#17562=ORIENTED_EDGE('',*,*,#12350,.F.);
#17563=ORIENTED_EDGE('',*,*,#12349,.F.);
#17564=ORIENTED_EDGE('',*,*,#12351,.F.);
#17565=ORIENTED_EDGE('',*,*,#12352,.T.);
#17566=ORIENTED_EDGE('',*,*,#12353,.F.);
#17567=ORIENTED_EDGE('',*,*,#12352,.F.);
#17568=ORIENTED_EDGE('',*,*,#12354,.F.);
#17569=ORIENTED_EDGE('',*,*,#12344,.T.);
#17570=ORIENTED_EDGE('',*,*,#12355,.F.);
#17571=ORIENTED_EDGE('',*,*,#12356,.F.);
#17572=ORIENTED_EDGE('',*,*,#12357,.F.);
#17573=ORIENTED_EDGE('',*,*,#12358,.T.);
#17574=ORIENTED_EDGE('',*,*,#12359,.F.);
#17575=ORIENTED_EDGE('',*,*,#12358,.F.);
#17576=ORIENTED_EDGE('',*,*,#12360,.F.);
#17577=ORIENTED_EDGE('',*,*,#12361,.T.);
#17578=ORIENTED_EDGE('',*,*,#12362,.F.);
#17579=ORIENTED_EDGE('',*,*,#12361,.F.);
#17580=ORIENTED_EDGE('',*,*,#12363,.F.);
#17581=ORIENTED_EDGE('',*,*,#12364,.T.);
#17582=ORIENTED_EDGE('',*,*,#12365,.F.);
#17583=ORIENTED_EDGE('',*,*,#12364,.F.);
#17584=ORIENTED_EDGE('',*,*,#12366,.F.);
#17585=ORIENTED_EDGE('',*,*,#12356,.T.);
#17586=ORIENTED_EDGE('',*,*,#12367,.F.);
#17587=ORIENTED_EDGE('',*,*,#12368,.F.);
#17588=ORIENTED_EDGE('',*,*,#12369,.F.);
#17589=ORIENTED_EDGE('',*,*,#12370,.T.);
#17590=ORIENTED_EDGE('',*,*,#12371,.F.);
#17591=ORIENTED_EDGE('',*,*,#12370,.F.);
#17592=ORIENTED_EDGE('',*,*,#12372,.F.);
#17593=ORIENTED_EDGE('',*,*,#12373,.T.);
#17594=ORIENTED_EDGE('',*,*,#12374,.F.);
#17595=ORIENTED_EDGE('',*,*,#12373,.F.);
#17596=ORIENTED_EDGE('',*,*,#12375,.F.);
#17597=ORIENTED_EDGE('',*,*,#12376,.T.);
#17598=ORIENTED_EDGE('',*,*,#12377,.F.);
#17599=ORIENTED_EDGE('',*,*,#12376,.F.);
#17600=ORIENTED_EDGE('',*,*,#12378,.F.);
#17601=ORIENTED_EDGE('',*,*,#12368,.T.);
#17602=ORIENTED_EDGE('',*,*,#12379,.F.);
#17603=ORIENTED_EDGE('',*,*,#12380,.F.);
#17604=ORIENTED_EDGE('',*,*,#12381,.F.);
#17605=ORIENTED_EDGE('',*,*,#12382,.T.);
#17606=ORIENTED_EDGE('',*,*,#12383,.F.);
#17607=ORIENTED_EDGE('',*,*,#12382,.F.);
#17608=ORIENTED_EDGE('',*,*,#12384,.F.);
#17609=ORIENTED_EDGE('',*,*,#12385,.T.);
#17610=ORIENTED_EDGE('',*,*,#12386,.F.);
#17611=ORIENTED_EDGE('',*,*,#12385,.F.);
#17612=ORIENTED_EDGE('',*,*,#12387,.F.);
#17613=ORIENTED_EDGE('',*,*,#12388,.T.);
#17614=ORIENTED_EDGE('',*,*,#12389,.F.);
#17615=ORIENTED_EDGE('',*,*,#12388,.F.);
#17616=ORIENTED_EDGE('',*,*,#12390,.F.);
#17617=ORIENTED_EDGE('',*,*,#12380,.T.);
#17618=ORIENTED_EDGE('',*,*,#12391,.F.);
#17619=ORIENTED_EDGE('',*,*,#12392,.F.);
#17620=ORIENTED_EDGE('',*,*,#12393,.T.);
#17621=ORIENTED_EDGE('',*,*,#12394,.F.);
#17622=ORIENTED_EDGE('',*,*,#12395,.F.);
#17623=ORIENTED_EDGE('',*,*,#12396,.F.);
#17624=ORIENTED_EDGE('',*,*,#12397,.F.);
#17625=ORIENTED_EDGE('',*,*,#12393,.F.);
#17626=ORIENTED_EDGE('',*,*,#12398,.F.);
#17627=ORIENTED_EDGE('',*,*,#12391,.T.);
#17628=ORIENTED_EDGE('',*,*,#12399,.F.);
#17629=ORIENTED_EDGE('',*,*,#12400,.F.);
#17630=ORIENTED_EDGE('',*,*,#12399,.T.);
#17631=ORIENTED_EDGE('',*,*,#12394,.T.);
#17632=ORIENTED_EDGE('',*,*,#12397,.T.);
#17633=ORIENTED_EDGE('',*,*,#12401,.F.);
#17634=ORIENTED_EDGE('',*,*,#12402,.F.);
#17635=ORIENTED_EDGE('',*,*,#12403,.F.);
#17636=ORIENTED_EDGE('',*,*,#12404,.T.);
#17637=ORIENTED_EDGE('',*,*,#12405,.F.);
#17638=ORIENTED_EDGE('',*,*,#12396,.T.);
#17639=ORIENTED_EDGE('',*,*,#12406,.F.);
#17640=ORIENTED_EDGE('',*,*,#12407,.T.);
#17641=ORIENTED_EDGE('',*,*,#12408,.F.);
#17642=ORIENTED_EDGE('',*,*,#12409,.T.);
#17643=ORIENTED_EDGE('',*,*,#12401,.T.);
#17644=ORIENTED_EDGE('',*,*,#12410,.F.);
#17645=ORIENTED_EDGE('',*,*,#12411,.F.);
#17646=ORIENTED_EDGE('',*,*,#12412,.F.);
#17647=ORIENTED_EDGE('',*,*,#12404,.F.);
#17648=ORIENTED_EDGE('',*,*,#12410,.T.);
#17649=ORIENTED_EDGE('',*,*,#12403,.T.);
#17650=ORIENTED_EDGE('',*,*,#12413,.F.);
#17651=ORIENTED_EDGE('',*,*,#12414,.T.);
#17652=ORIENTED_EDGE('',*,*,#12415,.T.);
#17653=ORIENTED_EDGE('',*,*,#12416,.T.);
#17654=ORIENTED_EDGE('',*,*,#12417,.F.);
#17655=ORIENTED_EDGE('',*,*,#12418,.T.);
#17656=ORIENTED_EDGE('',*,*,#12419,.T.);
#17657=ORIENTED_EDGE('',*,*,#12420,.T.);
#17658=ORIENTED_EDGE('',*,*,#12421,.F.);
#17659=ORIENTED_EDGE('',*,*,#12422,.F.);
#17660=ORIENTED_EDGE('',*,*,#12326,.T.);
#17661=ORIENTED_EDGE('',*,*,#12329,.T.);
#17662=ORIENTED_EDGE('',*,*,#12319,.T.);
#17663=ORIENTED_EDGE('',*,*,#12323,.T.);
#17664=ORIENTED_EDGE('',*,*,#12338,.T.);
#17665=ORIENTED_EDGE('',*,*,#12341,.T.);
#17666=ORIENTED_EDGE('',*,*,#12331,.T.);
#17667=ORIENTED_EDGE('',*,*,#12335,.T.);
#17668=ORIENTED_EDGE('',*,*,#12350,.T.);
#17669=ORIENTED_EDGE('',*,*,#12353,.T.);
#17670=ORIENTED_EDGE('',*,*,#12343,.T.);
#17671=ORIENTED_EDGE('',*,*,#12347,.T.);
#17672=ORIENTED_EDGE('',*,*,#12362,.T.);
#17673=ORIENTED_EDGE('',*,*,#12365,.T.);
#17674=ORIENTED_EDGE('',*,*,#12355,.T.);
#17675=ORIENTED_EDGE('',*,*,#12359,.T.);
#17676=ORIENTED_EDGE('',*,*,#12374,.T.);
#17677=ORIENTED_EDGE('',*,*,#12377,.T.);
#17678=ORIENTED_EDGE('',*,*,#12367,.T.);
#17679=ORIENTED_EDGE('',*,*,#12371,.T.);
#17680=ORIENTED_EDGE('',*,*,#12386,.T.);
#17681=ORIENTED_EDGE('',*,*,#12389,.T.);
#17682=ORIENTED_EDGE('',*,*,#12379,.T.);
#17683=ORIENTED_EDGE('',*,*,#12383,.T.);
#17684=ORIENTED_EDGE('',*,*,#12423,.T.);
#17685=ORIENTED_EDGE('',*,*,#12424,.T.);
#17686=ORIENTED_EDGE('',*,*,#12419,.F.);
#17687=ORIENTED_EDGE('',*,*,#12425,.T.);
#17688=ORIENTED_EDGE('',*,*,#12426,.T.);
#17689=ORIENTED_EDGE('',*,*,#12427,.F.);
#17690=ORIENTED_EDGE('',*,*,#12428,.T.);
#17691=ORIENTED_EDGE('',*,*,#12429,.F.);
#17692=ORIENTED_EDGE('',*,*,#12418,.F.);
#17693=ORIENTED_EDGE('',*,*,#12430,.F.);
#17694=ORIENTED_EDGE('',*,*,#12428,.F.);
#17695=ORIENTED_EDGE('',*,*,#12431,.F.);
#17696=ORIENTED_EDGE('',*,*,#12425,.F.);
#17697=ORIENTED_EDGE('',*,*,#12431,.T.);
#17698=ORIENTED_EDGE('',*,*,#12427,.T.);
#17699=ORIENTED_EDGE('',*,*,#12432,.T.);
#17700=ORIENTED_EDGE('',*,*,#12433,.F.);
#17701=ORIENTED_EDGE('',*,*,#12434,.F.);
#17702=ORIENTED_EDGE('',*,*,#12435,.T.);
#17703=ORIENTED_EDGE('',*,*,#12436,.T.);
#17704=ORIENTED_EDGE('',*,*,#12429,.T.);
#17705=ORIENTED_EDGE('',*,*,#12430,.T.);
#17706=ORIENTED_EDGE('',*,*,#12417,.T.);
#17707=ORIENTED_EDGE('',*,*,#12437,.T.);
#17708=ORIENTED_EDGE('',*,*,#12438,.T.);
#17709=ORIENTED_EDGE('',*,*,#12439,.T.);
#17710=ORIENTED_EDGE('',*,*,#12413,.T.);
#17711=ORIENTED_EDGE('',*,*,#12402,.T.);
#17712=ORIENTED_EDGE('',*,*,#12409,.F.);
#17713=ORIENTED_EDGE('',*,*,#12440,.F.);
#17714=ORIENTED_EDGE('',*,*,#12441,.F.);
#17715=ORIENTED_EDGE('',*,*,#12442,.F.);
#17716=ORIENTED_EDGE('',*,*,#12443,.F.);
#17717=ORIENTED_EDGE('',*,*,#12444,.F.);
#17718=ORIENTED_EDGE('',*,*,#12421,.T.);
#17719=ORIENTED_EDGE('',*,*,#12445,.T.);
#17720=ORIENTED_EDGE('',*,*,#12446,.T.);
#17721=ORIENTED_EDGE('',*,*,#12415,.F.);
#17722=ORIENTED_EDGE('',*,*,#12447,.F.);
#17723=ORIENTED_EDGE('',*,*,#12448,.F.);
#17724=ORIENTED_EDGE('',*,*,#12438,.F.);
#17725=ORIENTED_EDGE('',*,*,#12449,.T.);
#17726=ORIENTED_EDGE('',*,*,#12450,.F.);
#17727=ORIENTED_EDGE('',*,*,#12451,.F.);
#17728=ORIENTED_EDGE('',*,*,#12449,.F.);
#17729=ORIENTED_EDGE('',*,*,#12437,.F.);
#17730=ORIENTED_EDGE('',*,*,#12416,.F.);
#17731=ORIENTED_EDGE('',*,*,#12446,.F.);
#17732=ORIENTED_EDGE('',*,*,#12452,.T.);
#17733=ORIENTED_EDGE('',*,*,#12453,.F.);
#17734=ORIENTED_EDGE('',*,*,#12454,.T.);
#17735=ORIENTED_EDGE('',*,*,#12455,.F.);
#17736=ORIENTED_EDGE('',*,*,#12456,.F.);
#17737=ORIENTED_EDGE('',*,*,#12457,.F.);
#17738=ORIENTED_EDGE('',*,*,#12458,.F.);
#17739=ORIENTED_EDGE('',*,*,#12452,.F.);
#17740=ORIENTED_EDGE('',*,*,#12459,.F.);
#17741=ORIENTED_EDGE('',*,*,#12454,.F.);
#17742=ORIENTED_EDGE('',*,*,#12460,.F.);
#17743=ORIENTED_EDGE('',*,*,#12461,.F.);
#17744=ORIENTED_EDGE('',*,*,#12400,.T.);
#17745=ORIENTED_EDGE('',*,*,#12405,.T.);
#17746=ORIENTED_EDGE('',*,*,#12412,.T.);
#17747=ORIENTED_EDGE('',*,*,#12462,.F.);
#17748=ORIENTED_EDGE('',*,*,#12461,.T.);
#17749=ORIENTED_EDGE('',*,*,#12463,.T.);
#17750=ORIENTED_EDGE('',*,*,#12464,.F.);
#17751=ORIENTED_EDGE('',*,*,#12465,.F.);
#17752=ORIENTED_EDGE('',*,*,#12457,.T.);
#17753=ORIENTED_EDGE('',*,*,#12466,.F.);
#17754=ORIENTED_EDGE('',*,*,#12443,.T.);
#17755=ORIENTED_EDGE('',*,*,#12467,.T.);
#17756=ORIENTED_EDGE('',*,*,#12433,.T.);
#17757=ORIENTED_EDGE('',*,*,#12468,.T.);
#17758=ORIENTED_EDGE('',*,*,#12411,.T.);
#17759=ORIENTED_EDGE('',*,*,#12422,.T.);
#17760=ORIENTED_EDGE('',*,*,#12444,.T.);
#17761=ORIENTED_EDGE('',*,*,#12466,.T.);
#17762=ORIENTED_EDGE('',*,*,#12456,.T.);
#17763=ORIENTED_EDGE('',*,*,#12455,.T.);
#17764=ORIENTED_EDGE('',*,*,#12459,.T.);
#17765=ORIENTED_EDGE('',*,*,#12462,.T.);
#17766=ORIENTED_EDGE('',*,*,#12442,.T.);
#17767=ORIENTED_EDGE('',*,*,#12469,.T.);
#17768=ORIENTED_EDGE('',*,*,#12434,.T.);
#17769=ORIENTED_EDGE('',*,*,#12467,.F.);
#17770=ORIENTED_EDGE('',*,*,#12458,.T.);
#17771=ORIENTED_EDGE('',*,*,#12468,.F.);
#17772=ORIENTED_EDGE('',*,*,#12432,.F.);
#17773=ORIENTED_EDGE('',*,*,#12426,.F.);
#17774=ORIENTED_EDGE('',*,*,#12436,.F.);
#17775=ORIENTED_EDGE('',*,*,#12420,.F.);
#17776=ORIENTED_EDGE('',*,*,#12424,.F.);
#17777=ORIENTED_EDGE('',*,*,#12470,.F.);
#17778=ORIENTED_EDGE('',*,*,#12471,.F.);
#17779=ORIENTED_EDGE('',*,*,#12472,.F.);
#17780=ORIENTED_EDGE('',*,*,#12473,.F.);
#17781=ORIENTED_EDGE('',*,*,#12463,.F.);
#17782=ORIENTED_EDGE('',*,*,#12460,.T.);
#17783=ORIENTED_EDGE('',*,*,#12453,.T.);
#17784=ORIENTED_EDGE('',*,*,#12464,.T.);
#17785=ORIENTED_EDGE('',*,*,#12473,.T.);
#17786=ORIENTED_EDGE('',*,*,#12474,.F.);
#17787=ORIENTED_EDGE('',*,*,#12475,.F.);
#17788=ORIENTED_EDGE('',*,*,#12398,.T.);
#17789=ORIENTED_EDGE('',*,*,#12465,.T.);
#17790=ORIENTED_EDGE('',*,*,#12475,.T.);
#17791=ORIENTED_EDGE('',*,*,#12476,.T.);
#17792=ORIENTED_EDGE('',*,*,#12477,.T.);
#17793=ORIENTED_EDGE('',*,*,#12478,.T.);
#17794=ORIENTED_EDGE('',*,*,#12447,.T.);
#17795=ORIENTED_EDGE('',*,*,#12414,.F.);
#17796=ORIENTED_EDGE('',*,*,#12439,.F.);
#17797=ORIENTED_EDGE('',*,*,#12448,.T.);
#17798=ORIENTED_EDGE('',*,*,#12479,.T.);
#17799=ORIENTED_EDGE('',*,*,#12406,.T.);
#17800=ORIENTED_EDGE('',*,*,#12395,.T.);
#17801=ORIENTED_EDGE('',*,*,#12392,.T.);
#17802=ORIENTED_EDGE('',*,*,#12451,.T.);
#17803=ORIENTED_EDGE('',*,*,#12480,.T.);
#17804=ORIENTED_EDGE('',*,*,#12481,.F.);
#17805=ORIENTED_EDGE('',*,*,#12407,.F.);
#17806=ORIENTED_EDGE('',*,*,#12479,.F.);
#17807=ORIENTED_EDGE('',*,*,#12450,.T.);
#17808=ORIENTED_EDGE('',*,*,#12440,.T.);
#17809=ORIENTED_EDGE('',*,*,#12408,.T.);
#17810=ORIENTED_EDGE('',*,*,#12481,.T.);
#17811=ORIENTED_EDGE('',*,*,#12482,.F.);
#17812=ORIENTED_EDGE('',*,*,#12445,.F.);
#17813=ORIENTED_EDGE('',*,*,#12478,.F.);
#17814=ORIENTED_EDGE('',*,*,#12483,.T.);
#17815=ORIENTED_EDGE('',*,*,#12470,.T.);
#17816=ORIENTED_EDGE('',*,*,#12423,.F.);
#17817=ORIENTED_EDGE('',*,*,#12435,.F.);
#17818=ORIENTED_EDGE('',*,*,#12469,.F.);
#17819=ORIENTED_EDGE('',*,*,#12441,.T.);
#17820=ORIENTED_EDGE('',*,*,#12482,.T.);
#17821=ORIENTED_EDGE('',*,*,#12480,.F.);
#17822=ORIENTED_EDGE('',*,*,#12327,.T.);
#17823=ORIENTED_EDGE('',*,*,#12324,.T.);
#17824=ORIENTED_EDGE('',*,*,#12321,.T.);
#17825=ORIENTED_EDGE('',*,*,#12330,.T.);
#17826=ORIENTED_EDGE('',*,*,#12339,.T.);
#17827=ORIENTED_EDGE('',*,*,#12336,.T.);
#17828=ORIENTED_EDGE('',*,*,#12333,.T.);
#17829=ORIENTED_EDGE('',*,*,#12342,.T.);
#17830=ORIENTED_EDGE('',*,*,#12351,.T.);
#17831=ORIENTED_EDGE('',*,*,#12348,.T.);
#17832=ORIENTED_EDGE('',*,*,#12345,.T.);
#17833=ORIENTED_EDGE('',*,*,#12354,.T.);
#17834=ORIENTED_EDGE('',*,*,#12363,.T.);
#17835=ORIENTED_EDGE('',*,*,#12360,.T.);
#17836=ORIENTED_EDGE('',*,*,#12357,.T.);
#17837=ORIENTED_EDGE('',*,*,#12366,.T.);
#17838=ORIENTED_EDGE('',*,*,#12375,.T.);
#17839=ORIENTED_EDGE('',*,*,#12372,.T.);
#17840=ORIENTED_EDGE('',*,*,#12369,.T.);
#17841=ORIENTED_EDGE('',*,*,#12378,.T.);
#17842=ORIENTED_EDGE('',*,*,#12387,.T.);
#17843=ORIENTED_EDGE('',*,*,#12384,.T.);
#17844=ORIENTED_EDGE('',*,*,#12381,.T.);
#17845=ORIENTED_EDGE('',*,*,#12390,.T.);
#17846=ORIENTED_EDGE('',*,*,#12484,.T.);
#17847=ORIENTED_EDGE('',*,*,#12471,.T.);
#17848=ORIENTED_EDGE('',*,*,#12483,.F.);
#17849=ORIENTED_EDGE('',*,*,#12477,.F.);
#17850=ORIENTED_EDGE('',*,*,#12474,.T.);
#17851=ORIENTED_EDGE('',*,*,#12472,.T.);
#17852=ORIENTED_EDGE('',*,*,#12484,.F.);
#17853=ORIENTED_EDGE('',*,*,#12476,.F.);
#17854=ORIENTED_EDGE('',*,*,#12485,.T.);
#17855=ORIENTED_EDGE('',*,*,#12486,.T.);
#17856=ORIENTED_EDGE('',*,*,#12487,.T.);
#17857=ORIENTED_EDGE('',*,*,#12486,.F.);
#17858=ORIENTED_EDGE('',*,*,#12488,.T.);
#17859=ORIENTED_EDGE('',*,*,#12489,.T.);
#17860=ORIENTED_EDGE('',*,*,#12490,.T.);
#17861=ORIENTED_EDGE('',*,*,#12489,.F.);
#17862=ORIENTED_EDGE('',*,*,#12490,.F.);
#17863=ORIENTED_EDGE('',*,*,#12485,.F.);
#17864=ORIENTED_EDGE('',*,*,#12488,.F.);
#17865=ORIENTED_EDGE('',*,*,#12487,.F.);
#17866=ORIENTED_EDGE('',*,*,#12491,.T.);
#17867=ORIENTED_EDGE('',*,*,#12492,.T.);
#17868=ORIENTED_EDGE('',*,*,#12493,.T.);
#17869=ORIENTED_EDGE('',*,*,#12494,.T.);
#17870=ORIENTED_EDGE('',*,*,#12492,.F.);
#17871=ORIENTED_EDGE('',*,*,#12495,.F.);
#17872=ORIENTED_EDGE('',*,*,#12496,.F.);
#17873=ORIENTED_EDGE('',*,*,#12497,.F.);
#17874=ORIENTED_EDGE('',*,*,#12498,.T.);
#17875=ORIENTED_EDGE('',*,*,#12499,.T.);
#17876=ORIENTED_EDGE('',*,*,#12500,.T.);
#17877=ORIENTED_EDGE('',*,*,#12496,.T.);
#17878=ORIENTED_EDGE('',*,*,#12499,.F.);
#17879=ORIENTED_EDGE('',*,*,#12501,.F.);
#17880=ORIENTED_EDGE('',*,*,#12502,.F.);
#17881=ORIENTED_EDGE('',*,*,#12503,.F.);
#17882=ORIENTED_EDGE('',*,*,#12504,.T.);
#17883=ORIENTED_EDGE('',*,*,#12505,.T.);
#17884=ORIENTED_EDGE('',*,*,#12506,.T.);
#17885=ORIENTED_EDGE('',*,*,#12507,.T.);
#17886=ORIENTED_EDGE('',*,*,#12505,.F.);
#17887=ORIENTED_EDGE('',*,*,#12508,.F.);
#17888=ORIENTED_EDGE('',*,*,#12509,.F.);
#17889=ORIENTED_EDGE('',*,*,#12510,.F.);
#17890=ORIENTED_EDGE('',*,*,#12511,.T.);
#17891=ORIENTED_EDGE('',*,*,#12512,.T.);
#17892=ORIENTED_EDGE('',*,*,#12513,.T.);
#17893=ORIENTED_EDGE('',*,*,#12509,.T.);
#17894=ORIENTED_EDGE('',*,*,#12512,.F.);
#17895=ORIENTED_EDGE('',*,*,#12514,.F.);
#17896=ORIENTED_EDGE('',*,*,#12515,.F.);
#17897=ORIENTED_EDGE('',*,*,#12516,.F.);
#17898=ORIENTED_EDGE('',*,*,#12517,.T.);
#17899=ORIENTED_EDGE('',*,*,#12518,.T.);
#17900=ORIENTED_EDGE('',*,*,#12519,.T.);
#17901=ORIENTED_EDGE('',*,*,#12520,.T.);
#17902=ORIENTED_EDGE('',*,*,#12518,.F.);
#17903=ORIENTED_EDGE('',*,*,#12521,.F.);
#17904=ORIENTED_EDGE('',*,*,#12522,.F.);
#17905=ORIENTED_EDGE('',*,*,#12523,.F.);
#17906=ORIENTED_EDGE('',*,*,#12524,.T.);
#17907=ORIENTED_EDGE('',*,*,#12525,.T.);
#17908=ORIENTED_EDGE('',*,*,#12526,.T.);
#17909=ORIENTED_EDGE('',*,*,#12522,.T.);
#17910=ORIENTED_EDGE('',*,*,#12525,.F.);
#17911=ORIENTED_EDGE('',*,*,#12527,.F.);
#17912=ORIENTED_EDGE('',*,*,#12528,.F.);
#17913=ORIENTED_EDGE('',*,*,#12529,.F.);
#17914=ORIENTED_EDGE('',*,*,#12530,.T.);
#17915=ORIENTED_EDGE('',*,*,#12531,.T.);
#17916=ORIENTED_EDGE('',*,*,#12532,.T.);
#17917=ORIENTED_EDGE('',*,*,#12533,.T.);
#17918=ORIENTED_EDGE('',*,*,#12531,.F.);
#17919=ORIENTED_EDGE('',*,*,#12534,.F.);
#17920=ORIENTED_EDGE('',*,*,#12535,.F.);
#17921=ORIENTED_EDGE('',*,*,#12536,.F.);
#17922=ORIENTED_EDGE('',*,*,#12537,.T.);
#17923=ORIENTED_EDGE('',*,*,#12538,.T.);
#17924=ORIENTED_EDGE('',*,*,#12539,.T.);
#17925=ORIENTED_EDGE('',*,*,#12535,.T.);
#17926=ORIENTED_EDGE('',*,*,#12538,.F.);
#17927=ORIENTED_EDGE('',*,*,#12540,.F.);
#17928=ORIENTED_EDGE('',*,*,#12541,.F.);
#17929=ORIENTED_EDGE('',*,*,#12542,.F.);
#17930=ORIENTED_EDGE('',*,*,#12543,.T.);
#17931=ORIENTED_EDGE('',*,*,#12544,.T.);
#17932=ORIENTED_EDGE('',*,*,#12545,.T.);
#17933=ORIENTED_EDGE('',*,*,#12546,.T.);
#17934=ORIENTED_EDGE('',*,*,#12544,.F.);
#17935=ORIENTED_EDGE('',*,*,#12547,.F.);
#17936=ORIENTED_EDGE('',*,*,#12548,.F.);
#17937=ORIENTED_EDGE('',*,*,#12549,.F.);
#17938=ORIENTED_EDGE('',*,*,#12550,.T.);
#17939=ORIENTED_EDGE('',*,*,#12551,.T.);
#17940=ORIENTED_EDGE('',*,*,#12552,.T.);
#17941=ORIENTED_EDGE('',*,*,#12548,.T.);
#17942=ORIENTED_EDGE('',*,*,#12551,.F.);
#17943=ORIENTED_EDGE('',*,*,#12553,.F.);
#17944=ORIENTED_EDGE('',*,*,#12554,.F.);
#17945=ORIENTED_EDGE('',*,*,#12555,.F.);
#17946=ORIENTED_EDGE('',*,*,#12546,.F.);
#17947=ORIENTED_EDGE('',*,*,#12556,.F.);
#17948=ORIENTED_EDGE('',*,*,#12557,.F.);
#17949=ORIENTED_EDGE('',*,*,#12558,.F.);
#17950=ORIENTED_EDGE('',*,*,#12533,.F.);
#17951=ORIENTED_EDGE('',*,*,#12559,.F.);
#17952=ORIENTED_EDGE('',*,*,#12560,.F.);
#17953=ORIENTED_EDGE('',*,*,#12561,.F.);
#17954=ORIENTED_EDGE('',*,*,#12507,.F.);
#17955=ORIENTED_EDGE('',*,*,#12562,.F.);
#17956=ORIENTED_EDGE('',*,*,#12563,.F.);
#17957=ORIENTED_EDGE('',*,*,#12564,.F.);
#17958=ORIENTED_EDGE('',*,*,#12494,.F.);
#17959=ORIENTED_EDGE('',*,*,#12565,.F.);
#17960=ORIENTED_EDGE('',*,*,#12566,.F.);
#17961=ORIENTED_EDGE('',*,*,#12567,.F.);
#17962=ORIENTED_EDGE('',*,*,#12554,.T.);
#17963=ORIENTED_EDGE('',*,*,#12568,.F.);
#17964=ORIENTED_EDGE('',*,*,#12569,.T.);
#17965=ORIENTED_EDGE('',*,*,#12570,.F.);
#17966=ORIENTED_EDGE('',*,*,#12560,.T.);
#17967=ORIENTED_EDGE('',*,*,#12571,.F.);
#17968=ORIENTED_EDGE('',*,*,#12528,.T.);
#17969=ORIENTED_EDGE('',*,*,#12572,.F.);
#17970=ORIENTED_EDGE('',*,*,#12556,.T.);
#17971=ORIENTED_EDGE('',*,*,#12545,.F.);
#17972=ORIENTED_EDGE('',*,*,#12549,.T.);
#17973=ORIENTED_EDGE('',*,*,#12552,.F.);
#17974=ORIENTED_EDGE('',*,*,#12555,.T.);
#17975=ORIENTED_EDGE('',*,*,#12570,.T.);
#17976=ORIENTED_EDGE('',*,*,#12573,.T.);
#17977=ORIENTED_EDGE('',*,*,#12574,.T.);
#17978=ORIENTED_EDGE('',*,*,#12575,.T.);
#17979=ORIENTED_EDGE('',*,*,#12576,.T.);
#17980=ORIENTED_EDGE('',*,*,#12565,.T.);
#17981=ORIENTED_EDGE('',*,*,#12493,.F.);
#17982=ORIENTED_EDGE('',*,*,#12497,.T.);
#17983=ORIENTED_EDGE('',*,*,#12500,.F.);
#17984=ORIENTED_EDGE('',*,*,#12503,.T.);
#17985=ORIENTED_EDGE('',*,*,#12577,.T.);
#17986=ORIENTED_EDGE('',*,*,#12562,.T.);
#17987=ORIENTED_EDGE('',*,*,#12506,.F.);
#17988=ORIENTED_EDGE('',*,*,#12510,.T.);
#17989=ORIENTED_EDGE('',*,*,#12513,.F.);
#17990=ORIENTED_EDGE('',*,*,#12516,.T.);
#17991=ORIENTED_EDGE('',*,*,#12578,.T.);
#17992=ORIENTED_EDGE('',*,*,#12579,.T.);
#17993=ORIENTED_EDGE('',*,*,#12519,.F.);
#17994=ORIENTED_EDGE('',*,*,#12523,.T.);
#17995=ORIENTED_EDGE('',*,*,#12526,.F.);
#17996=ORIENTED_EDGE('',*,*,#12529,.T.);
#17997=ORIENTED_EDGE('',*,*,#12571,.T.);
#17998=ORIENTED_EDGE('',*,*,#12559,.T.);
#17999=ORIENTED_EDGE('',*,*,#12532,.F.);
#18000=ORIENTED_EDGE('',*,*,#12536,.T.);
#18001=ORIENTED_EDGE('',*,*,#12539,.F.);
#18002=ORIENTED_EDGE('',*,*,#12542,.T.);
#18003=ORIENTED_EDGE('',*,*,#12580,.T.);
#18004=ORIENTED_EDGE('',*,*,#12515,.T.);
#18005=ORIENTED_EDGE('',*,*,#12581,.F.);
#18006=ORIENTED_EDGE('',*,*,#12582,.T.);
#18007=ORIENTED_EDGE('',*,*,#12578,.F.);
#18008=ORIENTED_EDGE('',*,*,#12566,.T.);
#18009=ORIENTED_EDGE('',*,*,#12576,.F.);
#18010=ORIENTED_EDGE('',*,*,#12583,.T.);
#18011=ORIENTED_EDGE('',*,*,#12584,.F.);
#18012=ORIENTED_EDGE('',*,*,#12520,.F.);
#18013=ORIENTED_EDGE('',*,*,#12579,.F.);
#18014=ORIENTED_EDGE('',*,*,#12582,.F.);
#18015=ORIENTED_EDGE('',*,*,#12585,.F.);
#18016=ORIENTED_EDGE('',*,*,#12557,.T.);
#18017=ORIENTED_EDGE('',*,*,#12580,.F.);
#18018=ORIENTED_EDGE('',*,*,#12541,.T.);
#18019=ORIENTED_EDGE('',*,*,#12586,.F.);
#18020=ORIENTED_EDGE('',*,*,#12569,.F.);
#18021=ORIENTED_EDGE('',*,*,#12587,.F.);
#18022=ORIENTED_EDGE('',*,*,#12588,.F.);
#18023=ORIENTED_EDGE('',*,*,#12573,.F.);
#18024=ORIENTED_EDGE('',*,*,#12588,.T.);
#18025=ORIENTED_EDGE('',*,*,#12589,.F.);
#18026=ORIENTED_EDGE('',*,*,#12590,.F.);
#18027=ORIENTED_EDGE('',*,*,#12574,.F.);
#18028=ORIENTED_EDGE('',*,*,#12590,.T.);
#18029=ORIENTED_EDGE('',*,*,#12591,.F.);
#18030=ORIENTED_EDGE('',*,*,#12583,.F.);
#18031=ORIENTED_EDGE('',*,*,#12575,.F.);
#18032=ORIENTED_EDGE('',*,*,#12563,.T.);
#18033=ORIENTED_EDGE('',*,*,#12577,.F.);
#18034=ORIENTED_EDGE('',*,*,#12502,.T.);
#18035=ORIENTED_EDGE('',*,*,#12592,.F.);
#18036=ORIENTED_EDGE('',*,*,#12558,.T.);
#18037=ORIENTED_EDGE('',*,*,#12586,.T.);
#18038=ORIENTED_EDGE('',*,*,#12540,.T.);
#18039=ORIENTED_EDGE('',*,*,#12537,.F.);
#18040=ORIENTED_EDGE('',*,*,#12534,.T.);
#18041=ORIENTED_EDGE('',*,*,#12530,.F.);
#18042=ORIENTED_EDGE('',*,*,#12561,.T.);
#18043=ORIENTED_EDGE('',*,*,#12572,.T.);
#18044=ORIENTED_EDGE('',*,*,#12527,.T.);
#18045=ORIENTED_EDGE('',*,*,#12524,.F.);
#18046=ORIENTED_EDGE('',*,*,#12521,.T.);
#18047=ORIENTED_EDGE('',*,*,#12517,.F.);
#18048=ORIENTED_EDGE('',*,*,#12585,.T.);
#18049=ORIENTED_EDGE('',*,*,#12581,.T.);
#18050=ORIENTED_EDGE('',*,*,#12514,.T.);
#18051=ORIENTED_EDGE('',*,*,#12511,.F.);
#18052=ORIENTED_EDGE('',*,*,#12508,.T.);
#18053=ORIENTED_EDGE('',*,*,#12504,.F.);
#18054=ORIENTED_EDGE('',*,*,#12564,.T.);
#18055=ORIENTED_EDGE('',*,*,#12592,.T.);
#18056=ORIENTED_EDGE('',*,*,#12501,.T.);
#18057=ORIENTED_EDGE('',*,*,#12498,.F.);
#18058=ORIENTED_EDGE('',*,*,#12495,.T.);
#18059=ORIENTED_EDGE('',*,*,#12491,.F.);
#18060=ORIENTED_EDGE('',*,*,#12567,.T.);
#18061=ORIENTED_EDGE('',*,*,#12584,.T.);
#18062=ORIENTED_EDGE('',*,*,#12591,.T.);
#18063=ORIENTED_EDGE('',*,*,#12589,.T.);
#18064=ORIENTED_EDGE('',*,*,#12587,.T.);
#18065=ORIENTED_EDGE('',*,*,#12568,.T.);
#18066=ORIENTED_EDGE('',*,*,#12553,.T.);
#18067=ORIENTED_EDGE('',*,*,#12550,.F.);
#18068=ORIENTED_EDGE('',*,*,#12547,.T.);
#18069=ORIENTED_EDGE('',*,*,#12543,.F.);
#18070=ORIENTED_EDGE('',*,*,#12593,.T.);
#18071=ORIENTED_EDGE('',*,*,#12594,.T.);
#18072=ORIENTED_EDGE('',*,*,#12595,.T.);
#18073=ORIENTED_EDGE('',*,*,#12596,.T.);
#18074=ORIENTED_EDGE('',*,*,#12594,.F.);
#18075=ORIENTED_EDGE('',*,*,#12597,.F.);
#18076=ORIENTED_EDGE('',*,*,#12598,.F.);
#18077=ORIENTED_EDGE('',*,*,#12599,.F.);
#18078=ORIENTED_EDGE('',*,*,#12600,.T.);
#18079=ORIENTED_EDGE('',*,*,#12601,.T.);
#18080=ORIENTED_EDGE('',*,*,#12602,.T.);
#18081=ORIENTED_EDGE('',*,*,#12598,.T.);
#18082=ORIENTED_EDGE('',*,*,#12601,.F.);
#18083=ORIENTED_EDGE('',*,*,#12603,.F.);
#18084=ORIENTED_EDGE('',*,*,#12604,.F.);
#18085=ORIENTED_EDGE('',*,*,#12605,.F.);
#18086=ORIENTED_EDGE('',*,*,#12606,.T.);
#18087=ORIENTED_EDGE('',*,*,#12607,.T.);
#18088=ORIENTED_EDGE('',*,*,#12608,.T.);
#18089=ORIENTED_EDGE('',*,*,#12609,.T.);
#18090=ORIENTED_EDGE('',*,*,#12607,.F.);
#18091=ORIENTED_EDGE('',*,*,#12610,.F.);
#18092=ORIENTED_EDGE('',*,*,#12611,.F.);
#18093=ORIENTED_EDGE('',*,*,#12612,.F.);
#18094=ORIENTED_EDGE('',*,*,#12613,.T.);
#18095=ORIENTED_EDGE('',*,*,#12614,.T.);
#18096=ORIENTED_EDGE('',*,*,#12615,.T.);
#18097=ORIENTED_EDGE('',*,*,#12611,.T.);
#18098=ORIENTED_EDGE('',*,*,#12614,.F.);
#18099=ORIENTED_EDGE('',*,*,#12616,.F.);
#18100=ORIENTED_EDGE('',*,*,#12617,.F.);
#18101=ORIENTED_EDGE('',*,*,#12618,.F.);
#18102=ORIENTED_EDGE('',*,*,#12619,.T.);
#18103=ORIENTED_EDGE('',*,*,#12620,.T.);
#18104=ORIENTED_EDGE('',*,*,#12621,.T.);
#18105=ORIENTED_EDGE('',*,*,#12622,.T.);
#18106=ORIENTED_EDGE('',*,*,#12620,.F.);
#18107=ORIENTED_EDGE('',*,*,#12623,.F.);
#18108=ORIENTED_EDGE('',*,*,#12624,.F.);
#18109=ORIENTED_EDGE('',*,*,#12625,.F.);
#18110=ORIENTED_EDGE('',*,*,#12626,.T.);
#18111=ORIENTED_EDGE('',*,*,#12627,.T.);
#18112=ORIENTED_EDGE('',*,*,#12628,.T.);
#18113=ORIENTED_EDGE('',*,*,#12624,.T.);
#18114=ORIENTED_EDGE('',*,*,#12627,.F.);
#18115=ORIENTED_EDGE('',*,*,#12629,.F.);
#18116=ORIENTED_EDGE('',*,*,#12630,.F.);
#18117=ORIENTED_EDGE('',*,*,#12631,.F.);
#18118=ORIENTED_EDGE('',*,*,#12632,.T.);
#18119=ORIENTED_EDGE('',*,*,#12633,.T.);
#18120=ORIENTED_EDGE('',*,*,#12634,.T.);
#18121=ORIENTED_EDGE('',*,*,#12635,.T.);
#18122=ORIENTED_EDGE('',*,*,#12633,.F.);
#18123=ORIENTED_EDGE('',*,*,#12636,.F.);
#18124=ORIENTED_EDGE('',*,*,#12637,.F.);
#18125=ORIENTED_EDGE('',*,*,#12638,.F.);
#18126=ORIENTED_EDGE('',*,*,#12639,.T.);
#18127=ORIENTED_EDGE('',*,*,#12640,.T.);
#18128=ORIENTED_EDGE('',*,*,#12641,.T.);
#18129=ORIENTED_EDGE('',*,*,#12637,.T.);
#18130=ORIENTED_EDGE('',*,*,#12640,.F.);
#18131=ORIENTED_EDGE('',*,*,#12642,.F.);
#18132=ORIENTED_EDGE('',*,*,#12643,.F.);
#18133=ORIENTED_EDGE('',*,*,#12644,.F.);
#18134=ORIENTED_EDGE('',*,*,#12645,.T.);
#18135=ORIENTED_EDGE('',*,*,#12646,.T.);
#18136=ORIENTED_EDGE('',*,*,#12647,.T.);
#18137=ORIENTED_EDGE('',*,*,#12648,.T.);
#18138=ORIENTED_EDGE('',*,*,#12646,.F.);
#18139=ORIENTED_EDGE('',*,*,#12649,.F.);
#18140=ORIENTED_EDGE('',*,*,#12650,.F.);
#18141=ORIENTED_EDGE('',*,*,#12651,.F.);
#18142=ORIENTED_EDGE('',*,*,#12652,.T.);
#18143=ORIENTED_EDGE('',*,*,#12653,.T.);
#18144=ORIENTED_EDGE('',*,*,#12654,.T.);
#18145=ORIENTED_EDGE('',*,*,#12650,.T.);
#18146=ORIENTED_EDGE('',*,*,#12653,.F.);
#18147=ORIENTED_EDGE('',*,*,#12655,.F.);
#18148=ORIENTED_EDGE('',*,*,#12656,.F.);
#18149=ORIENTED_EDGE('',*,*,#12657,.F.);
#18150=ORIENTED_EDGE('',*,*,#12648,.F.);
#18151=ORIENTED_EDGE('',*,*,#12658,.F.);
#18152=ORIENTED_EDGE('',*,*,#12659,.F.);
#18153=ORIENTED_EDGE('',*,*,#12660,.F.);
#18154=ORIENTED_EDGE('',*,*,#12635,.F.);
#18155=ORIENTED_EDGE('',*,*,#12661,.F.);
#18156=ORIENTED_EDGE('',*,*,#12662,.F.);
#18157=ORIENTED_EDGE('',*,*,#12663,.F.);
#18158=ORIENTED_EDGE('',*,*,#12609,.F.);
#18159=ORIENTED_EDGE('',*,*,#12664,.F.);
#18160=ORIENTED_EDGE('',*,*,#12665,.F.);
#18161=ORIENTED_EDGE('',*,*,#12666,.F.);
#18162=ORIENTED_EDGE('',*,*,#12596,.F.);
#18163=ORIENTED_EDGE('',*,*,#12667,.F.);
#18164=ORIENTED_EDGE('',*,*,#12668,.F.);
#18165=ORIENTED_EDGE('',*,*,#12669,.F.);
#18166=ORIENTED_EDGE('',*,*,#12656,.T.);
#18167=ORIENTED_EDGE('',*,*,#12670,.F.);
#18168=ORIENTED_EDGE('',*,*,#12671,.T.);
#18169=ORIENTED_EDGE('',*,*,#12672,.F.);
#18170=ORIENTED_EDGE('',*,*,#12662,.T.);
#18171=ORIENTED_EDGE('',*,*,#12673,.F.);
#18172=ORIENTED_EDGE('',*,*,#12630,.T.);
#18173=ORIENTED_EDGE('',*,*,#12674,.F.);
#18174=ORIENTED_EDGE('',*,*,#12658,.T.);
#18175=ORIENTED_EDGE('',*,*,#12647,.F.);
#18176=ORIENTED_EDGE('',*,*,#12651,.T.);
#18177=ORIENTED_EDGE('',*,*,#12654,.F.);
#18178=ORIENTED_EDGE('',*,*,#12657,.T.);
#18179=ORIENTED_EDGE('',*,*,#12672,.T.);
#18180=ORIENTED_EDGE('',*,*,#12675,.T.);
#18181=ORIENTED_EDGE('',*,*,#12676,.T.);
#18182=ORIENTED_EDGE('',*,*,#12677,.T.);
#18183=ORIENTED_EDGE('',*,*,#12678,.T.);
#18184=ORIENTED_EDGE('',*,*,#12667,.T.);
#18185=ORIENTED_EDGE('',*,*,#12595,.F.);
#18186=ORIENTED_EDGE('',*,*,#12599,.T.);
#18187=ORIENTED_EDGE('',*,*,#12602,.F.);
#18188=ORIENTED_EDGE('',*,*,#12605,.T.);
#18189=ORIENTED_EDGE('',*,*,#12679,.T.);
#18190=ORIENTED_EDGE('',*,*,#12664,.T.);
#18191=ORIENTED_EDGE('',*,*,#12608,.F.);
#18192=ORIENTED_EDGE('',*,*,#12612,.T.);
#18193=ORIENTED_EDGE('',*,*,#12615,.F.);
#18194=ORIENTED_EDGE('',*,*,#12618,.T.);
#18195=ORIENTED_EDGE('',*,*,#12680,.T.);
#18196=ORIENTED_EDGE('',*,*,#12681,.T.);
#18197=ORIENTED_EDGE('',*,*,#12621,.F.);
#18198=ORIENTED_EDGE('',*,*,#12625,.T.);
#18199=ORIENTED_EDGE('',*,*,#12628,.F.);
#18200=ORIENTED_EDGE('',*,*,#12631,.T.);
#18201=ORIENTED_EDGE('',*,*,#12673,.T.);
#18202=ORIENTED_EDGE('',*,*,#12661,.T.);
#18203=ORIENTED_EDGE('',*,*,#12634,.F.);
#18204=ORIENTED_EDGE('',*,*,#12638,.T.);
#18205=ORIENTED_EDGE('',*,*,#12641,.F.);
#18206=ORIENTED_EDGE('',*,*,#12644,.T.);
#18207=ORIENTED_EDGE('',*,*,#12682,.T.);
#18208=ORIENTED_EDGE('',*,*,#12617,.T.);
#18209=ORIENTED_EDGE('',*,*,#12683,.F.);
#18210=ORIENTED_EDGE('',*,*,#12684,.T.);
#18211=ORIENTED_EDGE('',*,*,#12680,.F.);
#18212=ORIENTED_EDGE('',*,*,#12668,.T.);
#18213=ORIENTED_EDGE('',*,*,#12678,.F.);
#18214=ORIENTED_EDGE('',*,*,#12685,.T.);
#18215=ORIENTED_EDGE('',*,*,#12686,.F.);
#18216=ORIENTED_EDGE('',*,*,#12622,.F.);
#18217=ORIENTED_EDGE('',*,*,#12681,.F.);
#18218=ORIENTED_EDGE('',*,*,#12684,.F.);
#18219=ORIENTED_EDGE('',*,*,#12687,.F.);
#18220=ORIENTED_EDGE('',*,*,#12659,.T.);
#18221=ORIENTED_EDGE('',*,*,#12682,.F.);
#18222=ORIENTED_EDGE('',*,*,#12643,.T.);
#18223=ORIENTED_EDGE('',*,*,#12688,.F.);
#18224=ORIENTED_EDGE('',*,*,#12671,.F.);
#18225=ORIENTED_EDGE('',*,*,#12689,.F.);
#18226=ORIENTED_EDGE('',*,*,#12690,.F.);
#18227=ORIENTED_EDGE('',*,*,#12675,.F.);
#18228=ORIENTED_EDGE('',*,*,#12690,.T.);
#18229=ORIENTED_EDGE('',*,*,#12691,.F.);
#18230=ORIENTED_EDGE('',*,*,#12692,.F.);
#18231=ORIENTED_EDGE('',*,*,#12676,.F.);
#18232=ORIENTED_EDGE('',*,*,#12692,.T.);
#18233=ORIENTED_EDGE('',*,*,#12693,.F.);
#18234=ORIENTED_EDGE('',*,*,#12685,.F.);
#18235=ORIENTED_EDGE('',*,*,#12677,.F.);
#18236=ORIENTED_EDGE('',*,*,#12665,.T.);
#18237=ORIENTED_EDGE('',*,*,#12679,.F.);
#18238=ORIENTED_EDGE('',*,*,#12604,.T.);
#18239=ORIENTED_EDGE('',*,*,#12694,.F.);
#18240=ORIENTED_EDGE('',*,*,#12660,.T.);
#18241=ORIENTED_EDGE('',*,*,#12688,.T.);
#18242=ORIENTED_EDGE('',*,*,#12642,.T.);
#18243=ORIENTED_EDGE('',*,*,#12639,.F.);
#18244=ORIENTED_EDGE('',*,*,#12636,.T.);
#18245=ORIENTED_EDGE('',*,*,#12632,.F.);
#18246=ORIENTED_EDGE('',*,*,#12663,.T.);
#18247=ORIENTED_EDGE('',*,*,#12674,.T.);
#18248=ORIENTED_EDGE('',*,*,#12629,.T.);
#18249=ORIENTED_EDGE('',*,*,#12626,.F.);
#18250=ORIENTED_EDGE('',*,*,#12623,.T.);
#18251=ORIENTED_EDGE('',*,*,#12619,.F.);
#18252=ORIENTED_EDGE('',*,*,#12687,.T.);
#18253=ORIENTED_EDGE('',*,*,#12683,.T.);
#18254=ORIENTED_EDGE('',*,*,#12616,.T.);
#18255=ORIENTED_EDGE('',*,*,#12613,.F.);
#18256=ORIENTED_EDGE('',*,*,#12610,.T.);
#18257=ORIENTED_EDGE('',*,*,#12606,.F.);
#18258=ORIENTED_EDGE('',*,*,#12666,.T.);
#18259=ORIENTED_EDGE('',*,*,#12694,.T.);
#18260=ORIENTED_EDGE('',*,*,#12603,.T.);
#18261=ORIENTED_EDGE('',*,*,#12600,.F.);
#18262=ORIENTED_EDGE('',*,*,#12597,.T.);
#18263=ORIENTED_EDGE('',*,*,#12593,.F.);
#18264=ORIENTED_EDGE('',*,*,#12669,.T.);
#18265=ORIENTED_EDGE('',*,*,#12686,.T.);
#18266=ORIENTED_EDGE('',*,*,#12693,.T.);
#18267=ORIENTED_EDGE('',*,*,#12691,.T.);
#18268=ORIENTED_EDGE('',*,*,#12689,.T.);
#18269=ORIENTED_EDGE('',*,*,#12670,.T.);
#18270=ORIENTED_EDGE('',*,*,#12655,.T.);
#18271=ORIENTED_EDGE('',*,*,#12652,.F.);
#18272=ORIENTED_EDGE('',*,*,#12649,.T.);
#18273=ORIENTED_EDGE('',*,*,#12645,.F.);
#18274=ORIENTED_EDGE('',*,*,#12695,.T.);
#18275=ORIENTED_EDGE('',*,*,#12696,.T.);
#18276=ORIENTED_EDGE('',*,*,#12697,.T.);
#18277=ORIENTED_EDGE('',*,*,#12696,.F.);
#18278=ORIENTED_EDGE('',*,*,#12698,.T.);
#18279=ORIENTED_EDGE('',*,*,#12699,.F.);
#18280=ORIENTED_EDGE('',*,*,#12700,.T.);
#18281=ORIENTED_EDGE('',*,*,#12698,.F.);
#18282=ORIENTED_EDGE('',*,*,#12695,.F.);
#18283=ORIENTED_EDGE('',*,*,#12700,.F.);
#18284=ORIENTED_EDGE('',*,*,#12701,.F.);
#18285=ORIENTED_EDGE('',*,*,#12702,.T.);
#18286=ORIENTED_EDGE('',*,*,#12697,.F.);
#18287=ORIENTED_EDGE('',*,*,#12703,.T.);
#18288=ORIENTED_EDGE('',*,*,#12704,.T.);
#18289=ORIENTED_EDGE('',*,*,#12701,.T.);
#18290=ORIENTED_EDGE('',*,*,#12699,.T.);
#18291=ORIENTED_EDGE('',*,*,#12704,.F.);
#18292=ORIENTED_EDGE('',*,*,#12705,.F.);
#18293=ORIENTED_EDGE('',*,*,#12703,.F.);
#18294=ORIENTED_EDGE('',*,*,#12702,.F.);
#18295=ORIENTED_EDGE('',*,*,#12706,.T.);
#18296=ORIENTED_EDGE('',*,*,#12705,.T.);
#18297=ORIENTED_EDGE('',*,*,#12706,.F.);
#18298=ORIENTED_EDGE('',*,*,#12707,.T.);
#18299=ORIENTED_EDGE('',*,*,#12708,.T.);
#18300=ORIENTED_EDGE('',*,*,#12709,.T.);
#18301=ORIENTED_EDGE('',*,*,#12710,.F.);
#18302=ORIENTED_EDGE('',*,*,#12711,.F.);
#18303=ORIENTED_EDGE('',*,*,#12712,.T.);
#18304=ORIENTED_EDGE('',*,*,#12713,.T.);
#18305=ORIENTED_EDGE('',*,*,#12714,.F.);
#18306=ORIENTED_EDGE('',*,*,#12715,.F.);
#18307=ORIENTED_EDGE('',*,*,#12716,.T.);
#18308=ORIENTED_EDGE('',*,*,#12711,.T.);
#18309=ORIENTED_EDGE('',*,*,#12717,.F.);
#18310=ORIENTED_EDGE('',*,*,#12709,.F.);
#18311=ORIENTED_EDGE('',*,*,#12718,.F.);
#18312=ORIENTED_EDGE('',*,*,#12713,.F.);
#18313=ORIENTED_EDGE('',*,*,#12719,.F.);
#18314=ORIENTED_EDGE('',*,*,#12720,.F.);
#18315=ORIENTED_EDGE('',*,*,#12721,.F.);
#18316=ORIENTED_EDGE('',*,*,#12722,.F.);
#18317=ORIENTED_EDGE('',*,*,#12717,.T.);
#18318=ORIENTED_EDGE('',*,*,#12714,.T.);
#18319=ORIENTED_EDGE('',*,*,#12718,.T.);
#18320=ORIENTED_EDGE('',*,*,#12708,.F.);
#18321=ORIENTED_EDGE('',*,*,#12722,.T.);
#18322=ORIENTED_EDGE('',*,*,#12723,.F.);
#18323=ORIENTED_EDGE('',*,*,#12724,.F.);
#18324=ORIENTED_EDGE('',*,*,#12715,.T.);
#18325=ORIENTED_EDGE('',*,*,#12724,.T.);
#18326=ORIENTED_EDGE('',*,*,#12725,.F.);
#18327=ORIENTED_EDGE('',*,*,#12726,.F.);
#18328=ORIENTED_EDGE('',*,*,#12710,.T.);
#18329=ORIENTED_EDGE('',*,*,#12719,.T.);
#18330=ORIENTED_EDGE('',*,*,#12712,.F.);
#18331=ORIENTED_EDGE('',*,*,#12716,.F.);
#18332=ORIENTED_EDGE('',*,*,#12726,.T.);
#18333=ORIENTED_EDGE('',*,*,#12727,.F.);
#18334=ORIENTED_EDGE('',*,*,#12720,.T.);
#18335=ORIENTED_EDGE('',*,*,#12707,.F.);
#18336=ORIENTED_EDGE('',*,*,#12727,.T.);
#18337=ORIENTED_EDGE('',*,*,#12725,.T.);
#18338=ORIENTED_EDGE('',*,*,#12723,.T.);
#18339=ORIENTED_EDGE('',*,*,#12721,.T.);
#18340=ORIENTED_EDGE('',*,*,#12728,.T.);
#18341=ORIENTED_EDGE('',*,*,#12729,.T.);
#18342=ORIENTED_EDGE('',*,*,#12730,.T.);
#18343=ORIENTED_EDGE('',*,*,#12729,.F.);
#18344=ORIENTED_EDGE('',*,*,#12731,.T.);
#18345=ORIENTED_EDGE('',*,*,#12728,.F.);
#18346=ORIENTED_EDGE('',*,*,#12732,.T.);
#18347=ORIENTED_EDGE('',*,*,#12733,.T.);
#18348=ORIENTED_EDGE('',*,*,#12732,.F.);
#18349=ORIENTED_EDGE('',*,*,#12731,.F.);
#18350=ORIENTED_EDGE('',*,*,#12730,.F.);
#18351=ORIENTED_EDGE('',*,*,#12734,.T.);
#18352=ORIENTED_EDGE('',*,*,#12735,.T.);
#18353=ORIENTED_EDGE('',*,*,#12736,.T.);
#18354=ORIENTED_EDGE('',*,*,#12737,.T.);
#18355=ORIENTED_EDGE('',*,*,#12735,.F.);
#18356=ORIENTED_EDGE('',*,*,#12738,.T.);
#18357=ORIENTED_EDGE('',*,*,#12739,.T.);
#18358=ORIENTED_EDGE('',*,*,#12740,.T.);
#18359=ORIENTED_EDGE('',*,*,#12741,.T.);
#18360=ORIENTED_EDGE('',*,*,#12742,.T.);
#18361=ORIENTED_EDGE('',*,*,#12743,.T.);
#18362=ORIENTED_EDGE('',*,*,#12744,.T.);
#18363=ORIENTED_EDGE('',*,*,#12742,.F.);
#18364=ORIENTED_EDGE('',*,*,#12745,.T.);
#18365=ORIENTED_EDGE('',*,*,#12746,.T.);
#18366=ORIENTED_EDGE('',*,*,#12747,.T.);
#18367=ORIENTED_EDGE('',*,*,#12748,.T.);
#18368=ORIENTED_EDGE('',*,*,#12749,.T.);
#18369=ORIENTED_EDGE('',*,*,#12750,.T.);
#18370=ORIENTED_EDGE('',*,*,#12751,.T.);
#18371=ORIENTED_EDGE('',*,*,#12749,.F.);
#18372=ORIENTED_EDGE('',*,*,#12752,.T.);
#18373=ORIENTED_EDGE('',*,*,#12753,.T.);
#18374=ORIENTED_EDGE('',*,*,#12754,.T.);
#18375=ORIENTED_EDGE('',*,*,#12755,.T.);
#18376=ORIENTED_EDGE('',*,*,#12756,.T.);
#18377=ORIENTED_EDGE('',*,*,#12757,.T.);
#18378=ORIENTED_EDGE('',*,*,#12758,.T.);
#18379=ORIENTED_EDGE('',*,*,#12759,.T.);
#18380=ORIENTED_EDGE('',*,*,#12757,.F.);
#18381=ORIENTED_EDGE('',*,*,#12760,.T.);
#18382=ORIENTED_EDGE('',*,*,#12761,.T.);
#18383=ORIENTED_EDGE('',*,*,#12762,.T.);
#18384=ORIENTED_EDGE('',*,*,#12763,.T.);
#18385=ORIENTED_EDGE('',*,*,#12764,.T.);
#18386=ORIENTED_EDGE('',*,*,#12765,.T.);
#18387=ORIENTED_EDGE('',*,*,#12764,.F.);
#18388=ORIENTED_EDGE('',*,*,#12766,.T.);
#18389=ORIENTED_EDGE('',*,*,#12765,.F.);
#18390=ORIENTED_EDGE('',*,*,#12767,.F.);
#18391=ORIENTED_EDGE('',*,*,#12768,.F.);
#18392=ORIENTED_EDGE('',*,*,#12769,.F.);
#18393=ORIENTED_EDGE('',*,*,#12759,.F.);
#18394=ORIENTED_EDGE('',*,*,#12770,.F.);
#18395=ORIENTED_EDGE('',*,*,#12771,.F.);
#18396=ORIENTED_EDGE('',*,*,#12772,.F.);
#18397=ORIENTED_EDGE('',*,*,#12751,.F.);
#18398=ORIENTED_EDGE('',*,*,#12773,.F.);
#18399=ORIENTED_EDGE('',*,*,#12774,.F.);
#18400=ORIENTED_EDGE('',*,*,#12775,.F.);
#18401=ORIENTED_EDGE('',*,*,#12744,.F.);
#18402=ORIENTED_EDGE('',*,*,#12776,.F.);
#18403=ORIENTED_EDGE('',*,*,#12777,.F.);
#18404=ORIENTED_EDGE('',*,*,#12778,.F.);
#18405=ORIENTED_EDGE('',*,*,#12737,.F.);
#18406=ORIENTED_EDGE('',*,*,#12779,.F.);
#18407=ORIENTED_EDGE('',*,*,#12780,.T.);
#18408=ORIENTED_EDGE('',*,*,#12766,.F.);
#18409=ORIENTED_EDGE('',*,*,#12763,.F.);
#18410=ORIENTED_EDGE('',*,*,#12780,.F.);
#18411=ORIENTED_EDGE('',*,*,#12768,.T.);
#18412=ORIENTED_EDGE('',*,*,#12781,.T.);
#18413=ORIENTED_EDGE('',*,*,#12782,.F.);
#18414=ORIENTED_EDGE('',*,*,#12783,.F.);
#18415=ORIENTED_EDGE('',*,*,#12767,.T.);
#18416=ORIENTED_EDGE('',*,*,#12736,.F.);
#18417=ORIENTED_EDGE('',*,*,#12740,.F.);
#18418=ORIENTED_EDGE('',*,*,#12784,.F.);
#18419=ORIENTED_EDGE('',*,*,#12781,.F.);
#18420=ORIENTED_EDGE('',*,*,#12778,.T.);
#18421=ORIENTED_EDGE('',*,*,#12785,.T.);
#18422=ORIENTED_EDGE('',*,*,#12786,.F.);
#18423=ORIENTED_EDGE('',*,*,#12738,.F.);
#18424=ORIENTED_EDGE('',*,*,#12734,.F.);
#18425=ORIENTED_EDGE('',*,*,#12777,.T.);
#18426=ORIENTED_EDGE('',*,*,#12787,.T.);
#18427=ORIENTED_EDGE('',*,*,#12788,.F.);
#18428=ORIENTED_EDGE('',*,*,#12785,.F.);
#18429=ORIENTED_EDGE('',*,*,#12773,.T.);
#18430=ORIENTED_EDGE('',*,*,#12750,.F.);
#18431=ORIENTED_EDGE('',*,*,#12755,.F.);
#18432=ORIENTED_EDGE('',*,*,#12789,.F.);
#18433=ORIENTED_EDGE('',*,*,#12790,.F.);
#18434=ORIENTED_EDGE('',*,*,#12776,.T.);
#18435=ORIENTED_EDGE('',*,*,#12743,.F.);
#18436=ORIENTED_EDGE('',*,*,#12747,.F.);
#18437=ORIENTED_EDGE('',*,*,#12791,.F.);
#18438=ORIENTED_EDGE('',*,*,#12787,.F.);
#18439=ORIENTED_EDGE('',*,*,#12769,.T.);
#18440=ORIENTED_EDGE('',*,*,#12783,.T.);
#18441=ORIENTED_EDGE('',*,*,#12792,.F.);
#18442=ORIENTED_EDGE('',*,*,#12760,.F.);
#18443=ORIENTED_EDGE('',*,*,#12756,.F.);
#18444=ORIENTED_EDGE('',*,*,#12770,.T.);
#18445=ORIENTED_EDGE('',*,*,#12758,.F.);
#18446=ORIENTED_EDGE('',*,*,#12762,.F.);
#18447=ORIENTED_EDGE('',*,*,#12793,.F.);
#18448=ORIENTED_EDGE('',*,*,#12794,.F.);
#18449=ORIENTED_EDGE('',*,*,#12775,.T.);
#18450=ORIENTED_EDGE('',*,*,#12795,.T.);
#18451=ORIENTED_EDGE('',*,*,#12796,.F.);
#18452=ORIENTED_EDGE('',*,*,#12745,.F.);
#18453=ORIENTED_EDGE('',*,*,#12741,.F.);
#18454=ORIENTED_EDGE('',*,*,#12774,.T.);
#18455=ORIENTED_EDGE('',*,*,#12790,.T.);
#18456=ORIENTED_EDGE('',*,*,#12797,.F.);
#18457=ORIENTED_EDGE('',*,*,#12795,.F.);
#18458=ORIENTED_EDGE('',*,*,#12771,.T.);
#18459=ORIENTED_EDGE('',*,*,#12794,.T.);
#18460=ORIENTED_EDGE('',*,*,#12798,.F.);
#18461=ORIENTED_EDGE('',*,*,#12799,.F.);
#18462=ORIENTED_EDGE('',*,*,#12772,.T.);
#18463=ORIENTED_EDGE('',*,*,#12799,.T.);
#18464=ORIENTED_EDGE('',*,*,#12800,.F.);
#18465=ORIENTED_EDGE('',*,*,#12752,.F.);
#18466=ORIENTED_EDGE('',*,*,#12748,.F.);
#18467=ORIENTED_EDGE('',*,*,#12801,.T.);
#18468=ORIENTED_EDGE('',*,*,#12753,.F.);
#18469=ORIENTED_EDGE('',*,*,#12800,.T.);
#18470=ORIENTED_EDGE('',*,*,#12798,.T.);
#18471=ORIENTED_EDGE('',*,*,#12793,.T.);
#18472=ORIENTED_EDGE('',*,*,#12761,.F.);
#18473=ORIENTED_EDGE('',*,*,#12792,.T.);
#18474=ORIENTED_EDGE('',*,*,#12782,.T.);
#18475=ORIENTED_EDGE('',*,*,#12784,.T.);
#18476=ORIENTED_EDGE('',*,*,#12739,.F.);
#18477=ORIENTED_EDGE('',*,*,#12786,.T.);
#18478=ORIENTED_EDGE('',*,*,#12788,.T.);
#18479=ORIENTED_EDGE('',*,*,#12791,.T.);
#18480=ORIENTED_EDGE('',*,*,#12746,.F.);
#18481=ORIENTED_EDGE('',*,*,#12796,.T.);
#18482=ORIENTED_EDGE('',*,*,#12797,.T.);
#18483=ORIENTED_EDGE('',*,*,#12789,.T.);
#18484=ORIENTED_EDGE('',*,*,#12754,.F.);
#18485=ORIENTED_EDGE('',*,*,#12801,.F.);
#18486=ORIENTED_EDGE('',*,*,#12802,.F.);
#18487=ORIENTED_EDGE('',*,*,#12803,.T.);
#18488=ORIENTED_EDGE('',*,*,#12804,.T.);
#18489=ORIENTED_EDGE('',*,*,#12803,.F.);
#18490=ORIENTED_EDGE('',*,*,#12779,.T.);
#18491=ORIENTED_EDGE('',*,*,#12804,.F.);
#18492=ORIENTED_EDGE('',*,*,#12733,.F.);
#18493=ORIENTED_EDGE('',*,*,#12805,.T.);
#18494=ORIENTED_EDGE('',*,*,#12802,.T.);
#18495=ORIENTED_EDGE('',*,*,#12805,.F.);
#18496=TOROIDAL_SURFACE('',#19953,0.007725,0.000275);
#18497=TOROIDAL_SURFACE('',#19963,0.007725,0.000275);
#18498=TOROIDAL_SURFACE('',#20793,0.007725,0.000275);
#18499=TOROIDAL_SURFACE('',#20803,0.007725,0.000275);
#18500=TOROIDAL_SURFACE('',#21651,0.002775,0.000275);
#18501=TOROIDAL_SURFACE('',#21661,0.002775,0.000275);
#18502=TOROIDAL_SURFACE('',#22131,0.002775,0.000275);
#18503=TOROIDAL_SURFACE('',#22141,0.002775,0.000275);
#18504=TOROIDAL_SURFACE('',#22167,0.00144491053032732,8.6E-5);
#18505=TOROIDAL_SURFACE('',#22172,0.00144491053032732,8.6E-5);
#18506=TOROIDAL_SURFACE('',#22177,0.00144491053032732,8.6E-5);
#18507=TOROIDAL_SURFACE('',#22183,0.00144491053032732,8.6E-5);
#18508=TOROIDAL_SURFACE('',#22188,0.0017648321851312,0.001);
#18509=ADVANCED_FACE('',(#4793),#18496,.T.);
#18510=ADVANCED_FACE('',(#4794),#4281,.T.);
#18511=ADVANCED_FACE('',(#4795,#480),#590,.T.);
#18512=ADVANCED_FACE('',(#4796),#18497,.T.);
#18513=ADVANCED_FACE('',(#4797,#481),#591,.T.);
#18514=ADVANCED_FACE('',(#4798),#4282,.F.);
#18515=ADVANCED_FACE('',(#4799),#4283,.F.);
#18516=ADVANCED_FACE('',(#4800),#4284,.F.);
#18517=ADVANCED_FACE('',(#4801),#4285,.F.);
#18518=ADVANCED_FACE('',(#4802),#592,.F.);
#18519=ADVANCED_FACE('',(#4803),#4286,.F.);
#18520=ADVANCED_FACE('',(#4804),#4287,.F.);
#18521=ADVANCED_FACE('',(#4805),#4288,.F.);
#18522=ADVANCED_FACE('',(#4806),#593,.F.);
#18523=ADVANCED_FACE('',(#4807),#4289,.F.);
#18524=ADVANCED_FACE('',(#4808),#4290,.F.);
#18525=ADVANCED_FACE('',(#4809),#4291,.F.);
#18526=ADVANCED_FACE('',(#4810),#594,.F.);
#18527=ADVANCED_FACE('',(#4811),#4292,.F.);
#18528=ADVANCED_FACE('',(#4812),#4293,.F.);
#18529=ADVANCED_FACE('',(#4813),#4294,.F.);
#18530=ADVANCED_FACE('',(#4814),#595,.F.);
#18531=ADVANCED_FACE('',(#4815),#4295,.F.);
#18532=ADVANCED_FACE('',(#4816),#4296,.F.);
#18533=ADVANCED_FACE('',(#4817),#4297,.F.);
#18534=ADVANCED_FACE('',(#4818),#596,.F.);
#18535=ADVANCED_FACE('',(#4819),#597,.F.);
#18536=ADVANCED_FACE('',(#4820),#598,.F.);
#18537=ADVANCED_FACE('',(#4821),#599,.F.);
#18538=ADVANCED_FACE('',(#4822),#600,.F.);
#18539=ADVANCED_FACE('',(#4823),#4298,.F.);
#18540=ADVANCED_FACE('',(#4824),#4299,.F.);
#18541=ADVANCED_FACE('',(#4825),#601,.F.);
#18542=ADVANCED_FACE('',(#4826),#4300,.F.);
#18543=ADVANCED_FACE('',(#4827),#4301,.F.);
#18544=ADVANCED_FACE('',(#4828),#602,.F.);
#18545=ADVANCED_FACE('',(#4829),#4302,.F.);
#18546=ADVANCED_FACE('',(#4830),#4303,.T.);
#18547=ADVANCED_FACE('',(#4831),#603,.T.);
#18548=ADVANCED_FACE('',(#4832),#4304,.F.);
#18549=ADVANCED_FACE('',(#4833),#604,.T.);
#18550=ADVANCED_FACE('',(#4834),#605,.T.);
#18551=ADVANCED_FACE('',(#4835,#482),#606,.F.);
#18552=ADVANCED_FACE('',(#4836),#4305,.F.);
#18553=ADVANCED_FACE('',(#4837),#4306,.T.);
#18554=ADVANCED_FACE('',(#4838,#483),#607,.T.);
#18555=ADVANCED_FACE('',(#4839,#484),#4307,.T.);
#18556=ADVANCED_FACE('',(#4840),#608,.F.);
#18557=ADVANCED_FACE('',(#4841),#609,.T.);
#18558=ADVANCED_FACE('',(#4842),#610,.T.);
#18559=ADVANCED_FACE('',(#4843),#611,.T.);
#18560=ADVANCED_FACE('',(#4844),#612,.F.);
#18561=ADVANCED_FACE('',(#4845),#613,.T.);
#18562=ADVANCED_FACE('',(#4846),#4308,.F.);
#18563=ADVANCED_FACE('',(#4847),#614,.T.);
#18564=ADVANCED_FACE('',(#4848),#615,.T.);
#18565=ADVANCED_FACE('',(#4849),#616,.T.);
#18566=ADVANCED_FACE('',(#4850),#4309,.T.);
#18567=ADVANCED_FACE('',(#4851),#4310,.T.);
#18568=ADVANCED_FACE('',(#4852),#617,.T.);
#18569=ADVANCED_FACE('',(#4853,#485),#4311,.T.);
#18570=ADVANCED_FACE('',(#4854),#618,.F.);
#18571=ADVANCED_FACE('',(#4855),#619,.T.);
#18572=ADVANCED_FACE('',(#4856),#620,.T.);
#18573=ADVANCED_FACE('',(#4857),#621,.T.);
#18574=ADVANCED_FACE('',(#4858),#622,.F.);
#18575=ADVANCED_FACE('',(#4859),#623,.T.);
#18576=ADVANCED_FACE('',(#4860),#4312,.F.);
#18577=ADVANCED_FACE('',(#4861),#624,.T.);
#18578=ADVANCED_FACE('',(#4862),#625,.T.);
#18579=ADVANCED_FACE('',(#4863),#626,.T.);
#18580=ADVANCED_FACE('',(#4864),#4313,.T.);
#18581=ADVANCED_FACE('',(#4865),#4314,.T.);
#18582=ADVANCED_FACE('',(#4866),#627,.T.);
#18583=ADVANCED_FACE('',(#4867,#486),#4315,.T.);
#18584=ADVANCED_FACE('',(#4868),#628,.F.);
#18585=ADVANCED_FACE('',(#4869),#629,.T.);
#18586=ADVANCED_FACE('',(#4870),#630,.T.);
#18587=ADVANCED_FACE('',(#4871),#631,.T.);
#18588=ADVANCED_FACE('',(#4872),#632,.F.);
#18589=ADVANCED_FACE('',(#4873),#633,.T.);
#18590=ADVANCED_FACE('',(#4874),#4316,.F.);
#18591=ADVANCED_FACE('',(#4875),#634,.T.);
#18592=ADVANCED_FACE('',(#4876),#635,.T.);
#18593=ADVANCED_FACE('',(#4877),#636,.T.);
#18594=ADVANCED_FACE('',(#4878),#4317,.T.);
#18595=ADVANCED_FACE('',(#4879),#4318,.T.);
#18596=ADVANCED_FACE('',(#4880),#637,.T.);
#18597=ADVANCED_FACE('',(#4881,#487),#4319,.T.);
#18598=ADVANCED_FACE('',(#4882),#638,.F.);
#18599=ADVANCED_FACE('',(#4883),#639,.T.);
#18600=ADVANCED_FACE('',(#4884),#640,.T.);
#18601=ADVANCED_FACE('',(#4885),#641,.T.);
#18602=ADVANCED_FACE('',(#4886),#642,.F.);
#18603=ADVANCED_FACE('',(#4887),#643,.T.);
#18604=ADVANCED_FACE('',(#4888),#4320,.F.);
#18605=ADVANCED_FACE('',(#4889),#644,.T.);
#18606=ADVANCED_FACE('',(#4890),#645,.T.);
#18607=ADVANCED_FACE('',(#4891),#646,.T.);
#18608=ADVANCED_FACE('',(#4892),#4321,.T.);
#18609=ADVANCED_FACE('',(#4893),#4322,.T.);
#18610=ADVANCED_FACE('',(#4894),#647,.T.);
#18611=ADVANCED_FACE('',(#4895,#488),#4323,.T.);
#18612=ADVANCED_FACE('',(#4896),#648,.F.);
#18613=ADVANCED_FACE('',(#4897),#649,.T.);
#18614=ADVANCED_FACE('',(#4898),#650,.T.);
#18615=ADVANCED_FACE('',(#4899),#651,.T.);
#18616=ADVANCED_FACE('',(#4900),#652,.F.);
#18617=ADVANCED_FACE('',(#4901),#653,.T.);
#18618=ADVANCED_FACE('',(#4902),#4324,.F.);
#18619=ADVANCED_FACE('',(#4903),#654,.T.);
#18620=ADVANCED_FACE('',(#4904),#655,.T.);
#18621=ADVANCED_FACE('',(#4905),#656,.T.);
#18622=ADVANCED_FACE('',(#4906),#4325,.T.);
#18623=ADVANCED_FACE('',(#4907),#4326,.T.);
#18624=ADVANCED_FACE('',(#4908),#657,.T.);
#18625=ADVANCED_FACE('',(#4909,#489),#4327,.T.);
#18626=ADVANCED_FACE('',(#4910),#658,.F.);
#18627=ADVANCED_FACE('',(#4911),#659,.T.);
#18628=ADVANCED_FACE('',(#4912),#660,.T.);
#18629=ADVANCED_FACE('',(#4913),#661,.T.);
#18630=ADVANCED_FACE('',(#4914),#662,.F.);
#18631=ADVANCED_FACE('',(#4915),#663,.T.);
#18632=ADVANCED_FACE('',(#4916),#4328,.F.);
#18633=ADVANCED_FACE('',(#4917),#664,.T.);
#18634=ADVANCED_FACE('',(#4918),#665,.T.);
#18635=ADVANCED_FACE('',(#4919),#666,.T.);
#18636=ADVANCED_FACE('',(#4920),#4329,.T.);
#18637=ADVANCED_FACE('',(#4921),#4330,.T.);
#18638=ADVANCED_FACE('',(#4922),#667,.T.);
#18639=ADVANCED_FACE('',(#4923,#490),#4331,.T.);
#18640=ADVANCED_FACE('',(#4924),#668,.F.);
#18641=ADVANCED_FACE('',(#4925),#669,.T.);
#18642=ADVANCED_FACE('',(#4926),#670,.T.);
#18643=ADVANCED_FACE('',(#4927),#671,.T.);
#18644=ADVANCED_FACE('',(#4928),#672,.F.);
#18645=ADVANCED_FACE('',(#4929),#673,.T.);
#18646=ADVANCED_FACE('',(#4930),#4332,.F.);
#18647=ADVANCED_FACE('',(#4931),#674,.T.);
#18648=ADVANCED_FACE('',(#4932),#675,.T.);
#18649=ADVANCED_FACE('',(#4933),#676,.T.);
#18650=ADVANCED_FACE('',(#4934),#4333,.T.);
#18651=ADVANCED_FACE('',(#4935),#4334,.T.);
#18652=ADVANCED_FACE('',(#4936),#677,.T.);
#18653=ADVANCED_FACE('',(#4937,#491),#4335,.T.);
#18654=ADVANCED_FACE('',(#4938),#678,.F.);
#18655=ADVANCED_FACE('',(#4939),#679,.T.);
#18656=ADVANCED_FACE('',(#4940),#680,.T.);
#18657=ADVANCED_FACE('',(#4941),#681,.T.);
#18658=ADVANCED_FACE('',(#4942),#682,.F.);
#18659=ADVANCED_FACE('',(#4943),#683,.T.);
#18660=ADVANCED_FACE('',(#4944),#4336,.F.);
#18661=ADVANCED_FACE('',(#4945),#684,.T.);
#18662=ADVANCED_FACE('',(#4946),#685,.T.);
#18663=ADVANCED_FACE('',(#4947),#686,.T.);
#18664=ADVANCED_FACE('',(#4948),#4337,.T.);
#18665=ADVANCED_FACE('',(#4949),#4338,.T.);
#18666=ADVANCED_FACE('',(#4950),#687,.T.);
#18667=ADVANCED_FACE('',(#4951,#492),#688,.T.);
#18668=ADVANCED_FACE('',(#4952),#689,.T.);
#18669=ADVANCED_FACE('',(#4953),#690,.T.);
#18670=ADVANCED_FACE('',(#4954),#691,.T.);
#18671=ADVANCED_FACE('',(#4955),#692,.T.);
#18672=ADVANCED_FACE('',(#4956),#693,.T.);
#18673=ADVANCED_FACE('',(#4957),#694,.T.);
#18674=ADVANCED_FACE('',(#4958),#695,.T.);
#18675=ADVANCED_FACE('',(#4959,#493),#696,.T.);
#18676=ADVANCED_FACE('',(#4960,#494),#697,.T.);
#18677=ADVANCED_FACE('',(#4961,#495),#698,.T.);
#18678=ADVANCED_FACE('',(#4962,#496),#699,.T.);
#18679=ADVANCED_FACE('',(#4963,#497),#700,.T.);
#18680=ADVANCED_FACE('',(#4964,#498),#701,.T.);
#18681=ADVANCED_FACE('',(#4965,#499),#702,.T.);
#18682=ADVANCED_FACE('',(#4966,#500),#703,.T.);
#18683=ADVANCED_FACE('',(#4967),#704,.F.);
#18684=ADVANCED_FACE('',(#4968),#705,.F.);
#18685=ADVANCED_FACE('',(#4969),#706,.F.);
#18686=ADVANCED_FACE('',(#4970),#707,.F.);
#18687=ADVANCED_FACE('',(#4971),#708,.T.);
#18688=ADVANCED_FACE('',(#4972),#709,.T.);
#18689=ADVANCED_FACE('',(#4973),#710,.T.);
#18690=ADVANCED_FACE('',(#4974),#711,.T.);
#18691=ADVANCED_FACE('',(#4975),#712,.T.);
#18692=ADVANCED_FACE('',(#4976),#713,.T.);
#18693=ADVANCED_FACE('',(#4977),#714,.T.);
#18694=ADVANCED_FACE('',(#4978),#715,.F.);
#18695=ADVANCED_FACE('',(#4979),#716,.F.);
#18696=ADVANCED_FACE('',(#4980),#4339,.F.);
#18697=ADVANCED_FACE('',(#4981),#4340,.F.);
#18698=ADVANCED_FACE('',(#4982),#4341,.F.);
#18699=ADVANCED_FACE('',(#4983),#4342,.F.);
#18700=ADVANCED_FACE('',(#4984),#4343,.F.);
#18701=ADVANCED_FACE('',(#4985),#4344,.F.);
#18702=ADVANCED_FACE('',(#4986),#4345,.F.);
#18703=ADVANCED_FACE('',(#4987),#4346,.F.);
#18704=ADVANCED_FACE('',(#4988),#4347,.F.);
#18705=ADVANCED_FACE('',(#4989),#4348,.F.);
#18706=ADVANCED_FACE('',(#4990),#4349,.F.);
#18707=ADVANCED_FACE('',(#4991),#4350,.F.);
#18708=ADVANCED_FACE('',(#4992),#4351,.F.);
#18709=ADVANCED_FACE('',(#4993),#4352,.F.);
#18710=ADVANCED_FACE('',(#4994),#4353,.F.);
#18711=ADVANCED_FACE('',(#4995),#4354,.F.);
#18712=ADVANCED_FACE('',(#4996),#4355,.F.);
#18713=ADVANCED_FACE('',(#4997),#4356,.F.);
#18714=ADVANCED_FACE('',(#4998),#4357,.F.);
#18715=ADVANCED_FACE('',(#4999),#4358,.F.);
#18716=ADVANCED_FACE('',(#5000),#4359,.F.);
#18717=ADVANCED_FACE('',(#5001),#4360,.F.);
#18718=ADVANCED_FACE('',(#5002),#4361,.F.);
#18719=ADVANCED_FACE('',(#5003),#4362,.F.);
#18720=ADVANCED_FACE('',(#5004),#4363,.F.);
#18721=ADVANCED_FACE('',(#5005),#4364,.F.);
#18722=ADVANCED_FACE('',(#5006),#4365,.F.);
#18723=ADVANCED_FACE('',(#5007),#4366,.F.);
#18724=ADVANCED_FACE('',(#5008),#4367,.F.);
#18725=ADVANCED_FACE('',(#5009),#4368,.F.);
#18726=ADVANCED_FACE('',(#5010),#4369,.F.);
#18727=ADVANCED_FACE('',(#5011),#4370,.F.);
#18728=ADVANCED_FACE('',(#5012),#4371,.F.);
#18729=ADVANCED_FACE('',(#5013),#4372,.F.);
#18730=ADVANCED_FACE('',(#5014),#4373,.F.);
#18731=ADVANCED_FACE('',(#5015),#4374,.F.);
#18732=ADVANCED_FACE('',(#5016),#4375,.F.);
#18733=ADVANCED_FACE('',(#5017),#4376,.F.);
#18734=ADVANCED_FACE('',(#5018),#4377,.F.);
#18735=ADVANCED_FACE('',(#5019),#4378,.F.);
#18736=ADVANCED_FACE('',(#5020),#4379,.F.);
#18737=ADVANCED_FACE('',(#5021),#4380,.F.);
#18738=ADVANCED_FACE('',(#5022),#4381,.F.);
#18739=ADVANCED_FACE('',(#5023),#4382,.F.);
#18740=ADVANCED_FACE('',(#5024,#501),#717,.F.);
#18741=ADVANCED_FACE('',(#5025),#4383,.T.);
#18742=ADVANCED_FACE('',(#5026),#4384,.T.);
#18743=ADVANCED_FACE('',(#5027),#4385,.T.);
#18744=ADVANCED_FACE('',(#5028),#4386,.T.);
#18745=ADVANCED_FACE('',(#5029),#4387,.T.);
#18746=ADVANCED_FACE('',(#5030),#4388,.T.);
#18747=ADVANCED_FACE('',(#5031),#4389,.T.);
#18748=ADVANCED_FACE('',(#5032),#4390,.T.);
#18749=ADVANCED_FACE('',(#5033),#4391,.T.);
#18750=ADVANCED_FACE('',(#5034),#4392,.T.);
#18751=ADVANCED_FACE('',(#5035),#4393,.T.);
#18752=ADVANCED_FACE('',(#5036),#4394,.T.);
#18753=ADVANCED_FACE('',(#5037),#4395,.T.);
#18754=ADVANCED_FACE('',(#5038),#4396,.T.);
#18755=ADVANCED_FACE('',(#5039),#4397,.T.);
#18756=ADVANCED_FACE('',(#5040),#4398,.T.);
#18757=ADVANCED_FACE('',(#5041),#4399,.T.);
#18758=ADVANCED_FACE('',(#5042),#4400,.T.);
#18759=ADVANCED_FACE('',(#5043),#4401,.T.);
#18760=ADVANCED_FACE('',(#5044),#4402,.T.);
#18761=ADVANCED_FACE('',(#5045),#4403,.T.);
#18762=ADVANCED_FACE('',(#5046),#4404,.T.);
#18763=ADVANCED_FACE('',(#5047),#4405,.T.);
#18764=ADVANCED_FACE('',(#5048),#4406,.T.);
#18765=ADVANCED_FACE('',(#5049),#4407,.T.);
#18766=ADVANCED_FACE('',(#5050),#4408,.T.);
#18767=ADVANCED_FACE('',(#5051),#4409,.T.);
#18768=ADVANCED_FACE('',(#5052),#4410,.T.);
#18769=ADVANCED_FACE('',(#5053),#4411,.T.);
#18770=ADVANCED_FACE('',(#5054),#4412,.T.);
#18771=ADVANCED_FACE('',(#5055),#4413,.T.);
#18772=ADVANCED_FACE('',(#5056),#4414,.T.);
#18773=ADVANCED_FACE('',(#5057),#4415,.T.);
#18774=ADVANCED_FACE('',(#5058),#4416,.T.);
#18775=ADVANCED_FACE('',(#5059),#4417,.T.);
#18776=ADVANCED_FACE('',(#5060),#4418,.T.);
#18777=ADVANCED_FACE('',(#5061),#4419,.T.);
#18778=ADVANCED_FACE('',(#5062),#4420,.T.);
#18779=ADVANCED_FACE('',(#5063),#4421,.T.);
#18780=ADVANCED_FACE('',(#5064),#4422,.T.);
#18781=ADVANCED_FACE('',(#5065),#4423,.T.);
#18782=ADVANCED_FACE('',(#5066),#4424,.T.);
#18783=ADVANCED_FACE('',(#5067),#4425,.T.);
#18784=ADVANCED_FACE('',(#5068),#4426,.T.);
#18785=ADVANCED_FACE('',(#5069),#4427,.F.);
#18786=ADVANCED_FACE('',(#5070,#502),#718,.T.);
#18787=ADVANCED_FACE('',(#5071),#4428,.T.);
#18788=ADVANCED_FACE('',(#5072),#4429,.F.);
#18789=ADVANCED_FACE('',(#5073),#719,.F.);
#18790=ADVANCED_FACE('',(#5074),#4430,.T.);
#18791=ADVANCED_FACE('',(#5075),#4431,.T.);
#18792=ADVANCED_FACE('',(#5076),#4432,.T.);
#18793=ADVANCED_FACE('',(#5077),#720,.F.);
#18794=ADVANCED_FACE('',(#5078),#4433,.T.);
#18795=ADVANCED_FACE('',(#5079),#4434,.T.);
#18796=ADVANCED_FACE('',(#5080),#4435,.T.);
#18797=ADVANCED_FACE('',(#5081),#721,.F.);
#18798=ADVANCED_FACE('',(#5082),#4436,.T.);
#18799=ADVANCED_FACE('',(#5083),#4437,.T.);
#18800=ADVANCED_FACE('',(#5084),#722,.F.);
#18801=ADVANCED_FACE('',(#5085),#723,.F.);
#18802=ADVANCED_FACE('',(#5086),#724,.F.);
#18803=ADVANCED_FACE('',(#5087),#725,.F.);
#18804=ADVANCED_FACE('',(#5088),#4438,.T.);
#18805=ADVANCED_FACE('',(#5089),#4439,.T.);
#18806=ADVANCED_FACE('',(#5090),#4440,.T.);
#18807=ADVANCED_FACE('',(#5091),#4441,.T.);
#18808=ADVANCED_FACE('',(#5092),#726,.F.);
#18809=ADVANCED_FACE('',(#5093),#727,.F.);
#18810=ADVANCED_FACE('',(#5094),#728,.T.);
#18811=ADVANCED_FACE('',(#5095),#174,.F.);
#18812=ADVANCED_FACE('',(#5096),#729,.T.);
#18813=ADVANCED_FACE('',(#5097),#730,.T.);
#18814=ADVANCED_FACE('',(#5098),#175,.F.);
#18815=ADVANCED_FACE('',(#5099),#731,.T.);
#18816=ADVANCED_FACE('',(#5100),#732,.T.);
#18817=ADVANCED_FACE('',(#5101),#176,.F.);
#18818=ADVANCED_FACE('',(#5102),#733,.T.);
#18819=ADVANCED_FACE('',(#5103),#734,.T.);
#18820=ADVANCED_FACE('',(#5104),#735,.T.);
#18821=ADVANCED_FACE('',(#5105),#736,.T.);
#18822=ADVANCED_FACE('',(#5106,#503),#737,.T.);
#18823=ADVANCED_FACE('',(#5107),#4442,.F.);
#18824=ADVANCED_FACE('',(#5108),#4443,.F.);
#18825=ADVANCED_FACE('',(#5109),#177,.F.);
#18826=ADVANCED_FACE('',(#5110),#4444,.F.);
#18827=ADVANCED_FACE('',(#5111),#4445,.F.);
#18828=ADVANCED_FACE('',(#5112),#4446,.T.);
#18829=ADVANCED_FACE('',(#5113),#738,.F.);
#18830=ADVANCED_FACE('',(#5114,#504,#505,#506,#507),#739,.F.);
#18831=ADVANCED_FACE('',(#5115),#4447,.T.);
#18832=ADVANCED_FACE('',(#5116),#740,.F.);
#18833=ADVANCED_FACE('',(#5117),#741,.F.);
#18834=ADVANCED_FACE('',(#5118),#742,.T.);
#18835=ADVANCED_FACE('',(#5119),#743,.T.);
#18836=ADVANCED_FACE('',(#5120),#744,.T.);
#18837=ADVANCED_FACE('',(#5121),#745,.T.);
#18838=ADVANCED_FACE('',(#5122),#746,.T.);
#18839=ADVANCED_FACE('',(#5123),#4448,.F.);
#18840=ADVANCED_FACE('',(#5124),#747,.F.);
#18841=ADVANCED_FACE('',(#5125),#4449,.F.);
#18842=ADVANCED_FACE('',(#5126),#748,.F.);
#18843=ADVANCED_FACE('',(#5127),#4450,.F.);
#18844=ADVANCED_FACE('',(#5128),#749,.F.);
#18845=ADVANCED_FACE('',(#5129),#4451,.F.);
#18846=ADVANCED_FACE('',(#5130),#750,.F.);
#18847=ADVANCED_FACE('',(#5131),#751,.F.);
#18848=ADVANCED_FACE('',(#5132),#752,.T.);
#18849=ADVANCED_FACE('',(#5133),#753,.T.);
#18850=ADVANCED_FACE('',(#5134),#4452,.F.);
#18851=ADVANCED_FACE('',(#5135),#754,.T.);
#18852=ADVANCED_FACE('',(#5136),#755,.T.);
#18853=ADVANCED_FACE('',(#5137),#4453,.T.);
#18854=ADVANCED_FACE('',(#5138),#756,.T.);
#18855=ADVANCED_FACE('',(#5139),#4454,.T.);
#18856=ADVANCED_FACE('',(#5140),#757,.T.);
#18857=ADVANCED_FACE('',(#5141),#4455,.T.);
#18858=ADVANCED_FACE('',(#5142),#758,.T.);
#18859=ADVANCED_FACE('',(#5143),#759,.F.);
#18860=ADVANCED_FACE('',(#5144),#760,.F.);
#18861=ADVANCED_FACE('',(#5145),#4456,.T.);
#18862=ADVANCED_FACE('',(#5146),#761,.T.);
#18863=ADVANCED_FACE('',(#5147),#762,.F.);
#18864=ADVANCED_FACE('',(#5148),#763,.T.);
#18865=ADVANCED_FACE('',(#5149),#178,.T.);
#18866=ADVANCED_FACE('',(#5150,#508),#764,.T.);
#18867=ADVANCED_FACE('',(#5151),#4457,.T.);
#18868=ADVANCED_FACE('',(#5152),#179,.F.);
#18869=ADVANCED_FACE('',(#5153),#4458,.F.);
#18870=ADVANCED_FACE('',(#5154,#509),#765,.T.);
#18871=ADVANCED_FACE('',(#5155),#4459,.F.);
#18872=ADVANCED_FACE('',(#5156,#510),#766,.T.);
#18873=ADVANCED_FACE('',(#5157),#4460,.F.);
#18874=ADVANCED_FACE('',(#5158,#511),#767,.T.);
#18875=ADVANCED_FACE('',(#5159),#4461,.F.);
#18876=ADVANCED_FACE('',(#5160,#512),#768,.T.);
#18877=ADVANCED_FACE('',(#5161),#4462,.F.);
#18878=ADVANCED_FACE('',(#5162,#513,#514),#769,.T.);
#18879=ADVANCED_FACE('',(#5163),#4463,.F.);
#18880=ADVANCED_FACE('',(#5164,#515),#770,.T.);
#18881=ADVANCED_FACE('',(#5165,#516),#771,.T.);
#18882=ADVANCED_FACE('',(#5166),#772,.F.);
#18883=ADVANCED_FACE('',(#5167),#773,.F.);
#18884=ADVANCED_FACE('',(#5168),#774,.F.);
#18885=ADVANCED_FACE('',(#5169),#775,.T.);
#18886=ADVANCED_FACE('',(#5170),#18498,.T.);
#18887=ADVANCED_FACE('',(#5171),#4464,.T.);
#18888=ADVANCED_FACE('',(#5172,#517),#776,.T.);
#18889=ADVANCED_FACE('',(#5173),#18499,.T.);
#18890=ADVANCED_FACE('',(#5174,#518),#777,.T.);
#18891=ADVANCED_FACE('',(#5175),#4465,.F.);
#18892=ADVANCED_FACE('',(#5176),#778,.T.);
#18893=ADVANCED_FACE('',(#5177),#779,.F.);
#18894=ADVANCED_FACE('',(#5178),#4466,.T.);
#18895=ADVANCED_FACE('',(#5179),#780,.F.);
#18896=ADVANCED_FACE('',(#5180),#781,.T.);
#18897=ADVANCED_FACE('',(#5181),#782,.T.);
#18898=ADVANCED_FACE('',(#5182),#783,.T.);
#18899=ADVANCED_FACE('',(#5183),#784,.T.);
#18900=ADVANCED_FACE('',(#5184),#785,.T.);
#18901=ADVANCED_FACE('',(#5185),#786,.F.);
#18902=ADVANCED_FACE('',(#5186),#787,.T.);
#18903=ADVANCED_FACE('',(#5187),#4467,.T.);
#18904=ADVANCED_FACE('',(#5188),#788,.T.);
#18905=ADVANCED_FACE('',(#5189),#789,.F.);
#18906=ADVANCED_FACE('',(#5190),#790,.T.);
#18907=ADVANCED_FACE('',(#5191),#791,.T.);
#18908=ADVANCED_FACE('',(#5192),#792,.T.);
#18909=ADVANCED_FACE('',(#5193),#793,.T.);
#18910=ADVANCED_FACE('',(#5194),#4468,.T.);
#18911=ADVANCED_FACE('',(#5195),#4469,.T.);
#18912=ADVANCED_FACE('',(#5196),#794,.T.);
#18913=ADVANCED_FACE('',(#5197),#4470,.F.);
#18914=ADVANCED_FACE('',(#5198),#4471,.T.);
#18915=ADVANCED_FACE('',(#5199),#795,.T.);
#18916=ADVANCED_FACE('',(#5200),#4472,.F.);
#18917=ADVANCED_FACE('',(#5201),#4473,.F.);
#18918=ADVANCED_FACE('',(#5202),#4474,.F.);
#18919=ADVANCED_FACE('',(#5203),#796,.T.);
#18920=ADVANCED_FACE('',(#5204),#4475,.T.);
#18921=ADVANCED_FACE('',(#5205),#797,.T.);
#18922=ADVANCED_FACE('',(#5206),#4476,.F.);
#18923=ADVANCED_FACE('',(#5207),#4477,.F.);
#18924=ADVANCED_FACE('',(#5208),#4478,.F.);
#18925=ADVANCED_FACE('',(#5209),#798,.T.);
#18926=ADVANCED_FACE('',(#5210),#4479,.T.);
#18927=ADVANCED_FACE('',(#5211),#4480,.F.);
#18928=ADVANCED_FACE('',(#5212),#799,.T.);
#18929=ADVANCED_FACE('',(#5213),#4481,.T.);
#18930=ADVANCED_FACE('',(#5214),#800,.F.);
#18931=ADVANCED_FACE('',(#5215),#801,.T.);
#18932=ADVANCED_FACE('',(#5216),#4482,.F.);
#18933=ADVANCED_FACE('',(#5217),#4483,.F.);
#18934=ADVANCED_FACE('',(#5218),#4484,.F.);
#18935=ADVANCED_FACE('',(#5219),#802,.F.);
#18936=ADVANCED_FACE('',(#5220),#4485,.F.);
#18937=ADVANCED_FACE('',(#5221),#4486,.F.);
#18938=ADVANCED_FACE('',(#5222),#4487,.F.);
#18939=ADVANCED_FACE('',(#5223),#803,.F.);
#18940=ADVANCED_FACE('',(#5224),#4488,.F.);
#18941=ADVANCED_FACE('',(#5225),#4489,.F.);
#18942=ADVANCED_FACE('',(#5226),#4490,.F.);
#18943=ADVANCED_FACE('',(#5227),#804,.F.);
#18944=ADVANCED_FACE('',(#5228),#4491,.F.);
#18945=ADVANCED_FACE('',(#5229),#4492,.F.);
#18946=ADVANCED_FACE('',(#5230),#4493,.F.);
#18947=ADVANCED_FACE('',(#5231),#805,.F.);
#18948=ADVANCED_FACE('',(#5232),#4494,.F.);
#18949=ADVANCED_FACE('',(#5233),#4495,.F.);
#18950=ADVANCED_FACE('',(#5234),#4496,.F.);
#18951=ADVANCED_FACE('',(#5235),#806,.F.);
#18952=ADVANCED_FACE('',(#5236),#807,.F.);
#18953=ADVANCED_FACE('',(#5237),#808,.F.);
#18954=ADVANCED_FACE('',(#5238),#809,.F.);
#18955=ADVANCED_FACE('',(#5239),#810,.F.);
#18956=ADVANCED_FACE('',(#5240),#4497,.F.);
#18957=ADVANCED_FACE('',(#5241),#4498,.F.);
#18958=ADVANCED_FACE('',(#5242),#811,.F.);
#18959=ADVANCED_FACE('',(#5243),#4499,.F.);
#18960=ADVANCED_FACE('',(#5244),#4500,.F.);
#18961=ADVANCED_FACE('',(#5245),#812,.F.);
#18962=ADVANCED_FACE('',(#5246),#4501,.F.);
#18963=ADVANCED_FACE('',(#5247),#813,.T.);
#18964=ADVANCED_FACE('',(#5248),#4502,.T.);
#18965=ADVANCED_FACE('',(#5249),#814,.T.);
#18966=ADVANCED_FACE('',(#5250),#4503,.F.);
#18967=ADVANCED_FACE('',(#5251),#815,.T.);
#18968=ADVANCED_FACE('',(#5252),#4504,.T.);
#18969=ADVANCED_FACE('',(#5253),#4505,.T.);
#18970=ADVANCED_FACE('',(#5254),#4506,.T.);
#18971=ADVANCED_FACE('',(#5255),#4507,.T.);
#18972=ADVANCED_FACE('',(#5256),#4508,.T.);
#18973=ADVANCED_FACE('',(#5257),#4509,.T.);
#18974=ADVANCED_FACE('',(#5258),#4510,.T.);
#18975=ADVANCED_FACE('',(#5259),#4511,.T.);
#18976=ADVANCED_FACE('',(#5260),#4512,.T.);
#18977=ADVANCED_FACE('',(#5261),#4513,.T.);
#18978=ADVANCED_FACE('',(#5262),#4514,.T.);
#18979=ADVANCED_FACE('',(#5263),#4515,.T.);
#18980=ADVANCED_FACE('',(#5264),#816,.T.);
#18981=ADVANCED_FACE('',(#5265),#817,.T.);
#18982=ADVANCED_FACE('',(#5266),#818,.T.);
#18983=ADVANCED_FACE('',(#5267),#819,.T.);
#18984=ADVANCED_FACE('',(#5268),#820,.T.);
#18985=ADVANCED_FACE('',(#5269,#519,#520,#521,#522,#523),#821,.F.);
#18986=ADVANCED_FACE('',(#5270),#822,.T.);
#18987=ADVANCED_FACE('',(#5271,#524,#525,#526,#527,#528),#823,.T.);
#18988=ADVANCED_FACE('',(#5272),#824,.T.);
#18989=ADVANCED_FACE('',(#5273),#825,.T.);
#18990=ADVANCED_FACE('',(#5274),#826,.T.);
#18991=ADVANCED_FACE('',(#5275),#827,.T.);
#18992=ADVANCED_FACE('',(#5276),#828,.T.);
#18993=ADVANCED_FACE('',(#5277),#829,.T.);
#18994=ADVANCED_FACE('',(#5278),#830,.T.);
#18995=ADVANCED_FACE('',(#5279),#831,.T.);
#18996=ADVANCED_FACE('',(#5280),#832,.F.);
#18997=ADVANCED_FACE('',(#5281),#833,.F.);
#18998=ADVANCED_FACE('',(#5282),#834,.F.);
#18999=ADVANCED_FACE('',(#5283),#835,.F.);
#19000=ADVANCED_FACE('',(#5284,#529),#836,.T.);
#19001=ADVANCED_FACE('',(#5285),#837,.T.);
#19002=ADVANCED_FACE('',(#5286),#180,.T.);
#19003=ADVANCED_FACE('',(#5287,#530),#838,.T.);
#19004=ADVANCED_FACE('',(#5288),#4516,.T.);
#19005=ADVANCED_FACE('',(#5289),#181,.F.);
#19006=ADVANCED_FACE('',(#5290),#4517,.F.);
#19007=ADVANCED_FACE('',(#5291),#182,.F.);
#19008=ADVANCED_FACE('',(#5292,#531),#839,.T.);
#19009=ADVANCED_FACE('',(#5293),#183,.T.);
#19010=ADVANCED_FACE('',(#5294,#532),#840,.T.);
#19011=ADVANCED_FACE('',(#5295),#4518,.T.);
#19012=ADVANCED_FACE('',(#5296),#184,.F.);
#19013=ADVANCED_FACE('',(#5297),#4519,.F.);
#19014=ADVANCED_FACE('',(#5298),#4520,.F.);
#19015=ADVANCED_FACE('',(#5299),#4521,.F.);
#19016=ADVANCED_FACE('',(#5300),#4522,.F.);
#19017=ADVANCED_FACE('',(#5301),#4523,.F.);
#19018=ADVANCED_FACE('',(#5302),#4524,.F.);
#19019=ADVANCED_FACE('',(#5303,#533),#841,.T.);
#19020=ADVANCED_FACE('',(#5304),#842,.F.);
#19021=ADVANCED_FACE('',(#5305),#843,.F.);
#19022=ADVANCED_FACE('',(#5306),#844,.F.);
#19023=ADVANCED_FACE('',(#5307),#845,.F.);
#19024=ADVANCED_FACE('',(#5308),#846,.T.);
#19025=ADVANCED_FACE('',(#5309),#4525,.F.);
#19026=ADVANCED_FACE('',(#5310),#4526,.F.);
#19027=ADVANCED_FACE('',(#5311),#4527,.F.);
#19028=ADVANCED_FACE('',(#5312),#847,.F.);
#19029=ADVANCED_FACE('',(#5313),#4528,.F.);
#19030=ADVANCED_FACE('',(#5314),#4529,.F.);
#19031=ADVANCED_FACE('',(#5315),#4530,.F.);
#19032=ADVANCED_FACE('',(#5316),#848,.F.);
#19033=ADVANCED_FACE('',(#5317),#4531,.F.);
#19034=ADVANCED_FACE('',(#5318),#4532,.F.);
#19035=ADVANCED_FACE('',(#5319),#4533,.F.);
#19036=ADVANCED_FACE('',(#5320),#849,.F.);
#19037=ADVANCED_FACE('',(#5321),#4534,.F.);
#19038=ADVANCED_FACE('',(#5322),#4535,.F.);
#19039=ADVANCED_FACE('',(#5323),#4536,.F.);
#19040=ADVANCED_FACE('',(#5324),#850,.F.);
#19041=ADVANCED_FACE('',(#5325),#4537,.F.);
#19042=ADVANCED_FACE('',(#5326),#4538,.F.);
#19043=ADVANCED_FACE('',(#5327),#4539,.F.);
#19044=ADVANCED_FACE('',(#5328),#851,.F.);
#19045=ADVANCED_FACE('',(#5329),#852,.F.);
#19046=ADVANCED_FACE('',(#5330),#853,.F.);
#19047=ADVANCED_FACE('',(#5331),#854,.F.);
#19048=ADVANCED_FACE('',(#5332),#855,.F.);
#19049=ADVANCED_FACE('',(#5333),#4540,.F.);
#19050=ADVANCED_FACE('',(#5334),#4541,.F.);
#19051=ADVANCED_FACE('',(#5335),#856,.F.);
#19052=ADVANCED_FACE('',(#5336),#4542,.F.);
#19053=ADVANCED_FACE('',(#5337),#4543,.F.);
#19054=ADVANCED_FACE('',(#5338),#857,.F.);
#19055=ADVANCED_FACE('',(#5339),#4544,.F.);
#19056=ADVANCED_FACE('',(#5340),#858,.T.);
#19057=ADVANCED_FACE('',(#5341),#4545,.T.);
#19058=ADVANCED_FACE('',(#5342),#859,.T.);
#19059=ADVANCED_FACE('',(#5343),#4546,.F.);
#19060=ADVANCED_FACE('',(#5344),#860,.T.);
#19061=ADVANCED_FACE('',(#5345),#185,.T.);
#19062=ADVANCED_FACE('',(#5346),#186,.T.);
#19063=ADVANCED_FACE('',(#5347),#4547,.T.);
#19064=ADVANCED_FACE('',(#5348,#534),#861,.F.);
#19065=ADVANCED_FACE('',(#5349,#535),#862,.T.);
#19066=ADVANCED_FACE('',(#5350),#4548,.T.);
#19067=ADVANCED_FACE('',(#5351),#863,.F.);
#19068=ADVANCED_FACE('',(#5352),#864,.F.);
#19069=ADVANCED_FACE('',(#5353),#4549,.T.);
#19070=ADVANCED_FACE('',(#5354),#187,.T.);
#19071=ADVANCED_FACE('',(#5355),#865,.F.);
#19072=ADVANCED_FACE('',(#5356),#866,.T.);
#19073=ADVANCED_FACE('',(#5357),#867,.F.);
#19074=ADVANCED_FACE('',(#5358),#868,.F.);
#19075=ADVANCED_FACE('',(#5359),#869,.F.);
#19076=ADVANCED_FACE('',(#5360),#870,.F.);
#19077=ADVANCED_FACE('',(#5361),#871,.T.);
#19078=ADVANCED_FACE('',(#5362),#872,.F.);
#19079=ADVANCED_FACE('',(#5363),#873,.F.);
#19080=ADVANCED_FACE('',(#5364),#874,.F.);
#19081=ADVANCED_FACE('',(#5365),#875,.F.);
#19082=ADVANCED_FACE('',(#5366),#876,.F.);
#19083=ADVANCED_FACE('',(#5367),#877,.T.);
#19084=ADVANCED_FACE('',(#5368),#4550,.F.);
#19085=ADVANCED_FACE('',(#5369),#878,.T.);
#19086=ADVANCED_FACE('',(#5370),#879,.T.);
#19087=ADVANCED_FACE('',(#5371),#880,.T.);
#19088=ADVANCED_FACE('',(#5372),#881,.T.);
#19089=ADVANCED_FACE('',(#5373),#4551,.F.);
#19090=ADVANCED_FACE('',(#5374),#4552,.F.);
#19091=ADVANCED_FACE('',(#5375),#4553,.F.);
#19092=ADVANCED_FACE('',(#5376),#4554,.F.);
#19093=ADVANCED_FACE('',(#5377),#4555,.F.);
#19094=ADVANCED_FACE('',(#5378),#4556,.F.);
#19095=ADVANCED_FACE('',(#5379),#4557,.F.);
#19096=ADVANCED_FACE('',(#5380),#4558,.F.);
#19097=ADVANCED_FACE('',(#5381),#4559,.F.);
#19098=ADVANCED_FACE('',(#5382),#4560,.F.);
#19099=ADVANCED_FACE('',(#5383),#882,.F.);
#19100=ADVANCED_FACE('',(#5384),#883,.F.);
#19101=ADVANCED_FACE('',(#5385),#884,.F.);
#19102=ADVANCED_FACE('',(#5386),#885,.F.);
#19103=ADVANCED_FACE('',(#5387),#886,.T.);
#19104=ADVANCED_FACE('',(#5388),#887,.T.);
#19105=ADVANCED_FACE('',(#5389),#888,.T.);
#19106=ADVANCED_FACE('',(#5390),#4561,.F.);
#19107=ADVANCED_FACE('',(#5391),#889,.T.);
#19108=ADVANCED_FACE('',(#5392),#890,.T.);
#19109=ADVANCED_FACE('',(#5393,#536,#537,#538,#539,#540,#541,#542,#543,
#544,#545),#891,.T.);
#19110=ADVANCED_FACE('',(#5394,#546,#547,#548,#549,#550,#551,#552,#553,
#554,#555),#892,.F.);
#19111=ADVANCED_FACE('',(#5395),#893,.T.);
#19112=ADVANCED_FACE('',(#5396),#894,.F.);
#19113=ADVANCED_FACE('',(#5397),#4562,.T.);
#19114=ADVANCED_FACE('',(#5398),#895,.F.);
#19115=ADVANCED_FACE('',(#5399),#896,.T.);
#19116=ADVANCED_FACE('',(#5400),#897,.T.);
#19117=ADVANCED_FACE('',(#5401),#898,.T.);
#19118=ADVANCED_FACE('',(#5402),#899,.T.);
#19119=ADVANCED_FACE('',(#5403),#900,.T.);
#19120=ADVANCED_FACE('',(#5404),#4563,.F.);
#19121=ADVANCED_FACE('',(#5405),#4564,.F.);
#19122=ADVANCED_FACE('',(#5406),#4565,.F.);
#19123=ADVANCED_FACE('',(#5407),#901,.F.);
#19124=ADVANCED_FACE('',(#5408),#4566,.F.);
#19125=ADVANCED_FACE('',(#5409),#4567,.F.);
#19126=ADVANCED_FACE('',(#5410),#4568,.F.);
#19127=ADVANCED_FACE('',(#5411),#902,.F.);
#19128=ADVANCED_FACE('',(#5412),#4569,.F.);
#19129=ADVANCED_FACE('',(#5413),#4570,.F.);
#19130=ADVANCED_FACE('',(#5414),#4571,.F.);
#19131=ADVANCED_FACE('',(#5415),#903,.F.);
#19132=ADVANCED_FACE('',(#5416),#4572,.F.);
#19133=ADVANCED_FACE('',(#5417),#4573,.F.);
#19134=ADVANCED_FACE('',(#5418),#4574,.F.);
#19135=ADVANCED_FACE('',(#5419),#904,.F.);
#19136=ADVANCED_FACE('',(#5420),#4575,.F.);
#19137=ADVANCED_FACE('',(#5421),#4576,.F.);
#19138=ADVANCED_FACE('',(#5422),#4577,.F.);
#19139=ADVANCED_FACE('',(#5423),#905,.F.);
#19140=ADVANCED_FACE('',(#5424),#906,.F.);
#19141=ADVANCED_FACE('',(#5425),#907,.F.);
#19142=ADVANCED_FACE('',(#5426),#908,.F.);
#19143=ADVANCED_FACE('',(#5427),#909,.F.);
#19144=ADVANCED_FACE('',(#5428),#4578,.F.);
#19145=ADVANCED_FACE('',(#5429),#4579,.F.);
#19146=ADVANCED_FACE('',(#5430),#910,.F.);
#19147=ADVANCED_FACE('',(#5431),#4580,.F.);
#19148=ADVANCED_FACE('',(#5432),#4581,.F.);
#19149=ADVANCED_FACE('',(#5433),#911,.F.);
#19150=ADVANCED_FACE('',(#5434),#4582,.F.);
#19151=ADVANCED_FACE('',(#5435),#4583,.T.);
#19152=ADVANCED_FACE('',(#5436),#912,.T.);
#19153=ADVANCED_FACE('',(#5437),#4584,.F.);
#19154=ADVANCED_FACE('',(#5438),#913,.T.);
#19155=ADVANCED_FACE('',(#5439),#914,.T.);
#19156=ADVANCED_FACE('',(#5440,#556),#915,.F.);
#19157=ADVANCED_FACE('',(#5441),#4585,.F.);
#19158=ADVANCED_FACE('',(#5442),#4586,.T.);
#19159=ADVANCED_FACE('',(#5443,#557),#916,.T.);
#19160=ADVANCED_FACE('',(#5444),#917,.T.);
#19161=ADVANCED_FACE('',(#5445),#918,.F.);
#19162=ADVANCED_FACE('',(#5446),#919,.T.);
#19163=ADVANCED_FACE('',(#5447),#4587,.T.);
#19164=ADVANCED_FACE('',(#5448),#920,.T.);
#19165=ADVANCED_FACE('',(#5449),#921,.F.);
#19166=ADVANCED_FACE('',(#5450),#922,.T.);
#19167=ADVANCED_FACE('',(#5451),#923,.T.);
#19168=ADVANCED_FACE('',(#5452),#924,.T.);
#19169=ADVANCED_FACE('',(#5453),#4588,.F.);
#19170=ADVANCED_FACE('',(#5454),#4589,.F.);
#19171=ADVANCED_FACE('',(#5455),#4590,.F.);
#19172=ADVANCED_FACE('',(#5456),#4591,.F.);
#19173=ADVANCED_FACE('',(#5457),#4592,.F.);
#19174=ADVANCED_FACE('',(#5458),#4593,.F.);
#19175=ADVANCED_FACE('',(#5459),#4594,.F.);
#19176=ADVANCED_FACE('',(#5460),#4595,.F.);
#19177=ADVANCED_FACE('',(#5461),#4596,.F.);
#19178=ADVANCED_FACE('',(#5462),#4597,.F.);
#19179=ADVANCED_FACE('',(#5463),#4598,.F.);
#19180=ADVANCED_FACE('',(#5464),#4599,.F.);
#19181=ADVANCED_FACE('',(#5465),#4600,.F.);
#19182=ADVANCED_FACE('',(#5466),#4601,.F.);
#19183=ADVANCED_FACE('',(#5467),#4602,.F.);
#19184=ADVANCED_FACE('',(#5468),#4603,.F.);
#19185=ADVANCED_FACE('',(#5469),#4604,.F.);
#19186=ADVANCED_FACE('',(#5470),#4605,.F.);
#19187=ADVANCED_FACE('',(#5471),#4606,.F.);
#19188=ADVANCED_FACE('',(#5472),#4607,.F.);
#19189=ADVANCED_FACE('',(#5473),#4608,.F.);
#19190=ADVANCED_FACE('',(#5474),#4609,.F.);
#19191=ADVANCED_FACE('',(#5475),#4610,.F.);
#19192=ADVANCED_FACE('',(#5476),#4611,.F.);
#19193=ADVANCED_FACE('',(#5477),#4612,.F.);
#19194=ADVANCED_FACE('',(#5478),#4613,.F.);
#19195=ADVANCED_FACE('',(#5479),#4614,.F.);
#19196=ADVANCED_FACE('',(#5480),#4615,.F.);
#19197=ADVANCED_FACE('',(#5481),#4616,.F.);
#19198=ADVANCED_FACE('',(#5482),#4617,.F.);
#19199=ADVANCED_FACE('',(#5483),#4618,.F.);
#19200=ADVANCED_FACE('',(#5484),#4619,.F.);
#19201=ADVANCED_FACE('',(#5485),#4620,.F.);
#19202=ADVANCED_FACE('',(#5486),#4621,.F.);
#19203=ADVANCED_FACE('',(#5487),#4622,.F.);
#19204=ADVANCED_FACE('',(#5488),#4623,.F.);
#19205=ADVANCED_FACE('',(#5489),#4624,.F.);
#19206=ADVANCED_FACE('',(#5490),#4625,.F.);
#19207=ADVANCED_FACE('',(#5491),#4626,.F.);
#19208=ADVANCED_FACE('',(#5492),#4627,.F.);
#19209=ADVANCED_FACE('',(#5493),#4628,.F.);
#19210=ADVANCED_FACE('',(#5494),#4629,.F.);
#19211=ADVANCED_FACE('',(#5495),#4630,.F.);
#19212=ADVANCED_FACE('',(#5496),#4631,.F.);
#19213=ADVANCED_FACE('',(#5497,#558),#925,.T.);
#19214=ADVANCED_FACE('',(#5498),#4632,.T.);
#19215=ADVANCED_FACE('',(#5499),#4633,.T.);
#19216=ADVANCED_FACE('',(#5500),#4634,.T.);
#19217=ADVANCED_FACE('',(#5501),#4635,.T.);
#19218=ADVANCED_FACE('',(#5502),#4636,.T.);
#19219=ADVANCED_FACE('',(#5503),#4637,.T.);
#19220=ADVANCED_FACE('',(#5504),#4638,.T.);
#19221=ADVANCED_FACE('',(#5505),#4639,.T.);
#19222=ADVANCED_FACE('',(#5506),#4640,.T.);
#19223=ADVANCED_FACE('',(#5507),#4641,.T.);
#19224=ADVANCED_FACE('',(#5508),#4642,.T.);
#19225=ADVANCED_FACE('',(#5509),#4643,.T.);
#19226=ADVANCED_FACE('',(#5510),#4644,.T.);
#19227=ADVANCED_FACE('',(#5511),#4645,.T.);
#19228=ADVANCED_FACE('',(#5512),#4646,.T.);
#19229=ADVANCED_FACE('',(#5513),#4647,.T.);
#19230=ADVANCED_FACE('',(#5514),#4648,.T.);
#19231=ADVANCED_FACE('',(#5515),#4649,.T.);
#19232=ADVANCED_FACE('',(#5516),#4650,.T.);
#19233=ADVANCED_FACE('',(#5517),#4651,.T.);
#19234=ADVANCED_FACE('',(#5518),#4652,.T.);
#19235=ADVANCED_FACE('',(#5519),#4653,.T.);
#19236=ADVANCED_FACE('',(#5520),#4654,.T.);
#19237=ADVANCED_FACE('',(#5521),#4655,.T.);
#19238=ADVANCED_FACE('',(#5522),#4656,.T.);
#19239=ADVANCED_FACE('',(#5523),#4657,.T.);
#19240=ADVANCED_FACE('',(#5524),#4658,.T.);
#19241=ADVANCED_FACE('',(#5525),#4659,.T.);
#19242=ADVANCED_FACE('',(#5526),#4660,.T.);
#19243=ADVANCED_FACE('',(#5527),#4661,.T.);
#19244=ADVANCED_FACE('',(#5528),#4662,.T.);
#19245=ADVANCED_FACE('',(#5529),#4663,.T.);
#19246=ADVANCED_FACE('',(#5530),#4664,.T.);
#19247=ADVANCED_FACE('',(#5531),#4665,.T.);
#19248=ADVANCED_FACE('',(#5532),#4666,.T.);
#19249=ADVANCED_FACE('',(#5533),#4667,.T.);
#19250=ADVANCED_FACE('',(#5534),#4668,.T.);
#19251=ADVANCED_FACE('',(#5535),#4669,.T.);
#19252=ADVANCED_FACE('',(#5536),#4670,.T.);
#19253=ADVANCED_FACE('',(#5537),#4671,.T.);
#19254=ADVANCED_FACE('',(#5538),#4672,.T.);
#19255=ADVANCED_FACE('',(#5539),#4673,.T.);
#19256=ADVANCED_FACE('',(#5540),#4674,.T.);
#19257=ADVANCED_FACE('',(#5541),#4675,.T.);
#19258=ADVANCED_FACE('',(#5542),#4676,.F.);
#19259=ADVANCED_FACE('',(#5543,#559),#926,.F.);
#19260=ADVANCED_FACE('',(#5544),#4677,.T.);
#19261=ADVANCED_FACE('',(#5545),#4678,.F.);
#19262=ADVANCED_FACE('',(#5546),#18500,.T.);
#19263=ADVANCED_FACE('',(#5547),#4679,.F.);
#19264=ADVANCED_FACE('',(#5548,#560),#927,.T.);
#19265=ADVANCED_FACE('',(#5549),#18501,.T.);
#19266=ADVANCED_FACE('',(#5550,#561),#928,.T.);
#19267=ADVANCED_FACE('',(#5551),#4680,.T.);
#19268=ADVANCED_FACE('',(#5552),#4681,.F.);
#19269=ADVANCED_FACE('',(#5553),#4682,.F.);
#19270=ADVANCED_FACE('',(#5554),#4683,.F.);
#19271=ADVANCED_FACE('',(#5555),#929,.F.);
#19272=ADVANCED_FACE('',(#5556),#4684,.F.);
#19273=ADVANCED_FACE('',(#5557),#4685,.F.);
#19274=ADVANCED_FACE('',(#5558),#4686,.F.);
#19275=ADVANCED_FACE('',(#5559),#930,.F.);
#19276=ADVANCED_FACE('',(#5560),#4687,.F.);
#19277=ADVANCED_FACE('',(#5561),#4688,.F.);
#19278=ADVANCED_FACE('',(#5562),#4689,.F.);
#19279=ADVANCED_FACE('',(#5563),#931,.F.);
#19280=ADVANCED_FACE('',(#5564),#4690,.F.);
#19281=ADVANCED_FACE('',(#5565),#4691,.F.);
#19282=ADVANCED_FACE('',(#5566),#4692,.F.);
#19283=ADVANCED_FACE('',(#5567),#932,.F.);
#19284=ADVANCED_FACE('',(#5568),#4693,.F.);
#19285=ADVANCED_FACE('',(#5569),#4694,.F.);
#19286=ADVANCED_FACE('',(#5570),#4695,.F.);
#19287=ADVANCED_FACE('',(#5571),#933,.F.);
#19288=ADVANCED_FACE('',(#5572),#934,.F.);
#19289=ADVANCED_FACE('',(#5573),#935,.F.);
#19290=ADVANCED_FACE('',(#5574),#936,.F.);
#19291=ADVANCED_FACE('',(#5575),#937,.F.);
#19292=ADVANCED_FACE('',(#5576),#4696,.F.);
#19293=ADVANCED_FACE('',(#5577),#4697,.F.);
#19294=ADVANCED_FACE('',(#5578),#938,.F.);
#19295=ADVANCED_FACE('',(#5579),#4698,.F.);
#19296=ADVANCED_FACE('',(#5580),#4699,.F.);
#19297=ADVANCED_FACE('',(#5581),#939,.F.);
#19298=ADVANCED_FACE('',(#5582),#4700,.F.);
#19299=ADVANCED_FACE('',(#5583),#940,.T.);
#19300=ADVANCED_FACE('',(#5584),#4701,.T.);
#19301=ADVANCED_FACE('',(#5585),#941,.T.);
#19302=ADVANCED_FACE('',(#5586),#4702,.F.);
#19303=ADVANCED_FACE('',(#5587),#942,.T.);
#19304=ADVANCED_FACE('',(#5588),#943,.T.);
#19305=ADVANCED_FACE('',(#5589),#944,.F.);
#19306=ADVANCED_FACE('',(#5590),#945,.F.);
#19307=ADVANCED_FACE('',(#5591),#946,.T.);
#19308=ADVANCED_FACE('',(#5592),#4703,.T.);
#19309=ADVANCED_FACE('',(#5593),#947,.T.);
#19310=ADVANCED_FACE('',(#5594),#948,.T.);
#19311=ADVANCED_FACE('',(#5595),#949,.T.);
#19312=ADVANCED_FACE('',(#5596),#950,.T.);
#19313=ADVANCED_FACE('',(#5597),#4704,.T.);
#19314=ADVANCED_FACE('',(#5598),#951,.T.);
#19315=ADVANCED_FACE('',(#5599),#4705,.T.);
#19316=ADVANCED_FACE('',(#5600),#4706,.T.);
#19317=ADVANCED_FACE('',(#5601),#4707,.T.);
#19318=ADVANCED_FACE('',(#5602),#952,.T.);
#19319=ADVANCED_FACE('',(#5603),#4708,.T.);
#19320=ADVANCED_FACE('',(#5604),#4709,.T.);
#19321=ADVANCED_FACE('',(#5605),#4710,.T.);
#19322=ADVANCED_FACE('',(#5606),#953,.T.);
#19323=ADVANCED_FACE('',(#5607),#4711,.T.);
#19324=ADVANCED_FACE('',(#5608),#4712,.T.);
#19325=ADVANCED_FACE('',(#5609),#4713,.T.);
#19326=ADVANCED_FACE('',(#5610),#954,.T.);
#19327=ADVANCED_FACE('',(#5611),#4714,.T.);
#19328=ADVANCED_FACE('',(#5612,#562,#563,#564,#565,#566),#955,.F.);
#19329=ADVANCED_FACE('',(#5613),#4715,.T.);
#19330=ADVANCED_FACE('',(#5614),#4716,.F.);
#19331=ADVANCED_FACE('',(#5615),#4717,.F.);
#19332=ADVANCED_FACE('',(#5616),#4718,.F.);
#19333=ADVANCED_FACE('',(#5617),#4719,.F.);
#19334=ADVANCED_FACE('',(#5618),#956,.T.);
#19335=ADVANCED_FACE('',(#5619),#957,.T.);
#19336=ADVANCED_FACE('',(#5620),#958,.T.);
#19337=ADVANCED_FACE('',(#5621),#959,.T.);
#19338=ADVANCED_FACE('',(#5622),#960,.T.);
#19339=ADVANCED_FACE('',(#5623),#961,.T.);
#19340=ADVANCED_FACE('',(#5624),#962,.T.);
#19341=ADVANCED_FACE('',(#5625),#963,.T.);
#19342=ADVANCED_FACE('',(#5626,#567,#568,#569,#570,#571),#964,.T.);
#19343=ADVANCED_FACE('',(#5627),#4720,.F.);
#19344=ADVANCED_FACE('',(#5628),#4721,.F.);
#19345=ADVANCED_FACE('',(#5629),#4722,.F.);
#19346=ADVANCED_FACE('',(#5630),#965,.F.);
#19347=ADVANCED_FACE('',(#5631),#4723,.F.);
#19348=ADVANCED_FACE('',(#5632),#4724,.F.);
#19349=ADVANCED_FACE('',(#5633),#4725,.F.);
#19350=ADVANCED_FACE('',(#5634),#966,.F.);
#19351=ADVANCED_FACE('',(#5635),#4726,.F.);
#19352=ADVANCED_FACE('',(#5636),#4727,.F.);
#19353=ADVANCED_FACE('',(#5637),#4728,.F.);
#19354=ADVANCED_FACE('',(#5638),#967,.F.);
#19355=ADVANCED_FACE('',(#5639),#4729,.F.);
#19356=ADVANCED_FACE('',(#5640),#4730,.F.);
#19357=ADVANCED_FACE('',(#5641),#4731,.F.);
#19358=ADVANCED_FACE('',(#5642),#968,.F.);
#19359=ADVANCED_FACE('',(#5643),#4732,.F.);
#19360=ADVANCED_FACE('',(#5644),#4733,.F.);
#19361=ADVANCED_FACE('',(#5645),#4734,.F.);
#19362=ADVANCED_FACE('',(#5646),#969,.F.);
#19363=ADVANCED_FACE('',(#5647),#970,.F.);
#19364=ADVANCED_FACE('',(#5648),#971,.F.);
#19365=ADVANCED_FACE('',(#5649),#972,.F.);
#19366=ADVANCED_FACE('',(#5650),#973,.F.);
#19367=ADVANCED_FACE('',(#5651),#4735,.F.);
#19368=ADVANCED_FACE('',(#5652),#4736,.F.);
#19369=ADVANCED_FACE('',(#5653),#974,.F.);
#19370=ADVANCED_FACE('',(#5654),#4737,.F.);
#19371=ADVANCED_FACE('',(#5655),#4738,.F.);
#19372=ADVANCED_FACE('',(#5656),#975,.F.);
#19373=ADVANCED_FACE('',(#5657),#4739,.F.);
#19374=ADVANCED_FACE('',(#5658),#4740,.T.);
#19375=ADVANCED_FACE('',(#5659),#976,.T.);
#19376=ADVANCED_FACE('',(#5660),#4741,.F.);
#19377=ADVANCED_FACE('',(#5661),#977,.T.);
#19378=ADVANCED_FACE('',(#5662),#978,.T.);
#19379=ADVANCED_FACE('',(#5663),#979,.F.);
#19380=ADVANCED_FACE('',(#5664),#980,.F.);
#19381=ADVANCED_FACE('',(#5665),#981,.F.);
#19382=ADVANCED_FACE('',(#5666),#982,.F.);
#19383=ADVANCED_FACE('',(#5667),#983,.F.);
#19384=ADVANCED_FACE('',(#5668),#984,.F.);
#19385=ADVANCED_FACE('',(#5669),#985,.F.);
#19386=ADVANCED_FACE('',(#5670),#986,.F.);
#19387=ADVANCED_FACE('',(#5671),#987,.F.);
#19388=ADVANCED_FACE('',(#5672),#988,.F.);
#19389=ADVANCED_FACE('',(#5673),#989,.F.);
#19390=ADVANCED_FACE('',(#5674),#990,.F.);
#19391=ADVANCED_FACE('',(#5675),#991,.F.);
#19392=ADVANCED_FACE('',(#5676),#992,.F.);
#19393=ADVANCED_FACE('',(#5677),#993,.F.);
#19394=ADVANCED_FACE('',(#5678),#994,.F.);
#19395=ADVANCED_FACE('',(#5679),#995,.F.);
#19396=ADVANCED_FACE('',(#5680),#996,.F.);
#19397=ADVANCED_FACE('',(#5681),#997,.F.);
#19398=ADVANCED_FACE('',(#5682),#998,.F.);
#19399=ADVANCED_FACE('',(#5683),#999,.F.);
#19400=ADVANCED_FACE('',(#5684),#1000,.F.);
#19401=ADVANCED_FACE('',(#5685),#1001,.F.);
#19402=ADVANCED_FACE('',(#5686),#1002,.F.);
#19403=ADVANCED_FACE('',(#5687),#1003,.F.);
#19404=ADVANCED_FACE('',(#5688),#1004,.F.);
#19405=ADVANCED_FACE('',(#5689),#1005,.F.);
#19406=ADVANCED_FACE('',(#5690),#1006,.T.);
#19407=ADVANCED_FACE('',(#5691),#1007,.F.);
#19408=ADVANCED_FACE('',(#5692),#1008,.F.);
#19409=ADVANCED_FACE('',(#5693,#572,#573,#574,#575,#576,#577),#1009,.F.);
#19410=ADVANCED_FACE('',(#5694),#1010,.F.);
#19411=ADVANCED_FACE('',(#5695),#1011,.F.);
#19412=ADVANCED_FACE('',(#5696),#1012,.F.);
#19413=ADVANCED_FACE('',(#5697),#1013,.F.);
#19414=ADVANCED_FACE('',(#5698),#1014,.F.);
#19415=ADVANCED_FACE('',(#5699),#1015,.F.);
#19416=ADVANCED_FACE('',(#5700),#1016,.F.);
#19417=ADVANCED_FACE('',(#5701),#1017,.F.);
#19418=ADVANCED_FACE('',(#5702),#1018,.F.);
#19419=ADVANCED_FACE('',(#5703),#1019,.T.);
#19420=ADVANCED_FACE('',(#5704),#1020,.F.);
#19421=ADVANCED_FACE('',(#5705),#1021,.F.);
#19422=ADVANCED_FACE('',(#5706),#1022,.F.);
#19423=ADVANCED_FACE('',(#5707),#1023,.F.);
#19424=ADVANCED_FACE('',(#5708),#1024,.F.);
#19425=ADVANCED_FACE('',(#5709),#1025,.T.);
#19426=ADVANCED_FACE('',(#5710),#1026,.F.);
#19427=ADVANCED_FACE('',(#5711),#1027,.F.);
#19428=ADVANCED_FACE('',(#5712),#1028,.F.);
#19429=ADVANCED_FACE('',(#5713),#1029,.F.);
#19430=ADVANCED_FACE('',(#5714,#578,#579,#580,#581,#582,#583),#1030,.F.);
#19431=ADVANCED_FACE('',(#5715),#1031,.F.);
#19432=ADVANCED_FACE('',(#5716),#1032,.F.);
#19433=ADVANCED_FACE('',(#5717),#4742,.F.);
#19434=ADVANCED_FACE('',(#5718),#4743,.T.);
#19435=ADVANCED_FACE('',(#5719,#584),#1033,.F.);
#19436=ADVANCED_FACE('',(#5720,#585),#1034,.T.);
#19437=ADVANCED_FACE('',(#5721),#4744,.F.);
#19438=ADVANCED_FACE('',(#5722),#4745,.F.);
#19439=ADVANCED_FACE('',(#5723),#4746,.F.);
#19440=ADVANCED_FACE('',(#5724),#1035,.F.);
#19441=ADVANCED_FACE('',(#5725),#4747,.F.);
#19442=ADVANCED_FACE('',(#5726),#4748,.F.);
#19443=ADVANCED_FACE('',(#5727),#4749,.F.);
#19444=ADVANCED_FACE('',(#5728),#1036,.F.);
#19445=ADVANCED_FACE('',(#5729),#4750,.F.);
#19446=ADVANCED_FACE('',(#5730),#4751,.F.);
#19447=ADVANCED_FACE('',(#5731),#4752,.F.);
#19448=ADVANCED_FACE('',(#5732),#1037,.F.);
#19449=ADVANCED_FACE('',(#5733),#4753,.F.);
#19450=ADVANCED_FACE('',(#5734),#4754,.F.);
#19451=ADVANCED_FACE('',(#5735),#4755,.F.);
#19452=ADVANCED_FACE('',(#5736),#1038,.F.);
#19453=ADVANCED_FACE('',(#5737),#4756,.F.);
#19454=ADVANCED_FACE('',(#5738),#4757,.F.);
#19455=ADVANCED_FACE('',(#5739),#4758,.F.);
#19456=ADVANCED_FACE('',(#5740),#1039,.F.);
#19457=ADVANCED_FACE('',(#5741),#1040,.F.);
#19458=ADVANCED_FACE('',(#5742),#1041,.F.);
#19459=ADVANCED_FACE('',(#5743),#1042,.F.);
#19460=ADVANCED_FACE('',(#5744),#1043,.F.);
#19461=ADVANCED_FACE('',(#5745),#4759,.F.);
#19462=ADVANCED_FACE('',(#5746),#4760,.F.);
#19463=ADVANCED_FACE('',(#5747),#1044,.F.);
#19464=ADVANCED_FACE('',(#5748),#4761,.F.);
#19465=ADVANCED_FACE('',(#5749),#4762,.F.);
#19466=ADVANCED_FACE('',(#5750),#1045,.F.);
#19467=ADVANCED_FACE('',(#5751),#4763,.F.);
#19468=ADVANCED_FACE('',(#5752),#1046,.T.);
#19469=ADVANCED_FACE('',(#5753),#4764,.T.);
#19470=ADVANCED_FACE('',(#5754),#1047,.T.);
#19471=ADVANCED_FACE('',(#5755),#4765,.F.);
#19472=ADVANCED_FACE('',(#5756),#1048,.T.);
#19473=ADVANCED_FACE('',(#5757),#4766,.F.);
#19474=ADVANCED_FACE('',(#5758),#4767,.F.);
#19475=ADVANCED_FACE('',(#5759),#4768,.F.);
#19476=ADVANCED_FACE('',(#5760),#1049,.F.);
#19477=ADVANCED_FACE('',(#5761),#4769,.F.);
#19478=ADVANCED_FACE('',(#5762),#4770,.F.);
#19479=ADVANCED_FACE('',(#5763),#4771,.F.);
#19480=ADVANCED_FACE('',(#5764),#1050,.F.);
#19481=ADVANCED_FACE('',(#5765),#4772,.F.);
#19482=ADVANCED_FACE('',(#5766),#4773,.F.);
#19483=ADVANCED_FACE('',(#5767),#4774,.F.);
#19484=ADVANCED_FACE('',(#5768),#1051,.F.);
#19485=ADVANCED_FACE('',(#5769),#4775,.F.);
#19486=ADVANCED_FACE('',(#5770),#4776,.F.);
#19487=ADVANCED_FACE('',(#5771),#4777,.F.);
#19488=ADVANCED_FACE('',(#5772),#1052,.F.);
#19489=ADVANCED_FACE('',(#5773),#4778,.F.);
#19490=ADVANCED_FACE('',(#5774),#4779,.F.);
#19491=ADVANCED_FACE('',(#5775),#4780,.F.);
#19492=ADVANCED_FACE('',(#5776),#1053,.F.);
#19493=ADVANCED_FACE('',(#5777),#1054,.F.);
#19494=ADVANCED_FACE('',(#5778),#1055,.F.);
#19495=ADVANCED_FACE('',(#5779),#1056,.F.);
#19496=ADVANCED_FACE('',(#5780),#1057,.F.);
#19497=ADVANCED_FACE('',(#5781),#4781,.F.);
#19498=ADVANCED_FACE('',(#5782),#4782,.F.);
#19499=ADVANCED_FACE('',(#5783),#1058,.F.);
#19500=ADVANCED_FACE('',(#5784),#4783,.F.);
#19501=ADVANCED_FACE('',(#5785),#4784,.F.);
#19502=ADVANCED_FACE('',(#5786),#1059,.F.);
#19503=ADVANCED_FACE('',(#5787),#4785,.F.);
#19504=ADVANCED_FACE('',(#5788),#1060,.T.);
#19505=ADVANCED_FACE('',(#5789),#4786,.T.);
#19506=ADVANCED_FACE('',(#5790),#1061,.T.);
#19507=ADVANCED_FACE('',(#5791),#4787,.F.);
#19508=ADVANCED_FACE('',(#5792),#1062,.T.);
#19509=ADVANCED_FACE('',(#5793),#18502,.T.);
#19510=ADVANCED_FACE('',(#5794),#4788,.F.);
#19511=ADVANCED_FACE('',(#5795,#586),#1063,.T.);
#19512=ADVANCED_FACE('',(#5796),#18503,.T.);
#19513=ADVANCED_FACE('',(#5797,#587),#1064,.T.);
#19514=ADVANCED_FACE('',(#5798),#4789,.T.);
#19515=ADVANCED_FACE('',(#5799),#1065,.T.);
#19516=ADVANCED_FACE('',(#5800),#1066,.F.);
#19517=ADVANCED_FACE('',(#5801),#4790,.T.);
#19518=ADVANCED_FACE('',(#5802),#1067,.F.);
#19519=ADVANCED_FACE('',(#5803),#1068,.T.);
#19520=ADVANCED_FACE('',(#5804),#1069,.T.);
#19521=ADVANCED_FACE('',(#5805),#1070,.T.);
#19522=ADVANCED_FACE('',(#5806),#1071,.T.);
#19523=ADVANCED_FACE('',(#5807),#1072,.T.);
#19524=ADVANCED_FACE('',(#5808),#188,.T.);
#19525=ADVANCED_FACE('',(#5809),#4791,.T.);
#19526=ADVANCED_FACE('',(#5810),#1073,.T.);
#19527=ADVANCED_FACE('',(#5811),#18504,.T.);
#19528=ADVANCED_FACE('',(#5812),#189,.F.);
#19529=ADVANCED_FACE('',(#5813),#18505,.T.);
#19530=ADVANCED_FACE('',(#5814),#190,.F.);
#19531=ADVANCED_FACE('',(#5815),#18506,.T.);
#19532=ADVANCED_FACE('',(#5816),#191,.F.);
#19533=ADVANCED_FACE('',(#5817),#18507,.T.);
#19534=ADVANCED_FACE('',(#5818),#192,.F.);
#19535=ADVANCED_FACE('',(#5819),#18508,.T.);
#19536=ADVANCED_FACE('',(#5820,#588),#155,.T.);
#19537=ADVANCED_FACE('',(#5821),#193,.T.);
#19538=ADVANCED_FACE('',(#5822),#194,.T.);
#19539=ADVANCED_FACE('',(#5823),#1074,.T.);
#19540=ADVANCED_FACE('',(#5824),#1075,.T.);
#19541=ADVANCED_FACE('',(#5825),#195,.T.);
#19542=ADVANCED_FACE('',(#5826),#1076,.T.);
#19543=ADVANCED_FACE('',(#5827),#1077,.T.);
#19544=ADVANCED_FACE('',(#5828),#1078,.T.);
#19545=ADVANCED_FACE('',(#5829),#1079,.T.);
#19546=ADVANCED_FACE('',(#5830),#1080,.T.);
#19547=ADVANCED_FACE('',(#5831),#196,.T.);
#19548=ADVANCED_FACE('',(#5832),#197,.T.);
#19549=ADVANCED_FACE('',(#5833),#1081,.T.);
#19550=ADVANCED_FACE('',(#5834),#198,.F.);
#19551=ADVANCED_FACE('',(#5835),#4792,.T.);
#19552=ADVANCED_FACE('',(#5836,#589),#1082,.T.);
#19553=ADVANCED_FACE('',(#5837),#199,.T.);
#19554=CLOSED_SHELL('',(#18509,#18510,#18511,#18512,#18513,#18514));
#19555=CLOSED_SHELL('',(#18515,#18516,#18517,#18518,#18519,#18520,#18521,
#18522,#18523,#18524,#18525,#18526,#18527,#18528,#18529,#18530,#18531,#18532,
#18533,#18534,#18535,#18536,#18537,#18538,#18539,#18540,#18541,#18542,#18543,
#18544,#18545,#18546,#18547,#18548,#18549,#18550));
#19556=CLOSED_SHELL('',(#18551,#18552,#18553,#18554));
#19557=CLOSED_SHELL('',(#18555,#18556,#18557,#18558,#18559,#18560,#18561,
#18562,#18563,#18564,#18565,#18566,#18567,#18568,#18569,#18570,#18571,#18572,
#18573,#18574,#18575,#18576,#18577,#18578,#18579,#18580,#18581,#18582,#18583,
#18584,#18585,#18586,#18587,#18588,#18589,#18590,#18591,#18592,#18593,#18594,
#18595,#18596,#18597,#18598,#18599,#18600,#18601,#18602,#18603,#18604,#18605,
#18606,#18607,#18608,#18609,#18610,#18611,#18612,#18613,#18614,#18615,#18616,
#18617,#18618,#18619,#18620,#18621,#18622,#18623,#18624,#18625,#18626,#18627,
#18628,#18629,#18630,#18631,#18632,#18633,#18634,#18635,#18636,#18637,#18638,
#18639,#18640,#18641,#18642,#18643,#18644,#18645,#18646,#18647,#18648,#18649,
#18650,#18651,#18652,#18653,#18654,#18655,#18656,#18657,#18658,#18659,#18660,
#18661,#18662,#18663,#18664,#18665,#18666,#18667,#18668,#18669,#18670,#18671,
#18672,#18673,#18674,#18675,#18676,#18677,#18678,#18679,#18680,#18681,#18682,
#18683,#18684,#18685,#18686,#18687,#18688,#18689,#18690,#18691,#18692,#18693,
#18694,#18695));
#19558=CLOSED_SHELL('',(#18696,#18697,#18698,#18699,#18700,#18701,#18702,
#18703,#18704,#18705,#18706,#18707,#18708,#18709,#18710,#18711,#18712,#18713,
#18714,#18715,#18716,#18717,#18718,#18719,#18720,#18721,#18722,#18723,#18724,
#18725,#18726,#18727,#18728,#18729,#18730,#18731,#18732,#18733,#18734,#18735,
#18736,#18737,#18738,#18739,#18740,#18741,#18742,#18743,#18744,#18745,#18746,
#18747,#18748,#18749,#18750,#18751,#18752,#18753,#18754,#18755,#18756,#18757,
#18758,#18759,#18760,#18761,#18762,#18763,#18764,#18765,#18766,#18767,#18768,
#18769,#18770,#18771,#18772,#18773,#18774,#18775,#18776,#18777,#18778,#18779,
#18780,#18781,#18782,#18783,#18784,#18785,#18786,#18787,#18788));
#19559=CLOSED_SHELL('',(#18789,#18790,#18791,#18792,#18793,#18794,#18795,
#18796,#18797,#18798,#18799,#18800,#18801,#18802,#18803,#18804,#18805,#18806,
#18807,#18808,#18809,#18810,#18811,#18812,#18813,#18814,#18815,#18816,#18817,
#18818,#18819,#18820,#18821,#18822,#18823,#18824,#18825,#18826,#18827,#18828,
#18829,#18830,#18831,#18832,#18833,#18834,#18835,#18836,#18837,#18838,#18839,
#18840,#18841,#18842,#18843,#18844,#18845,#18846,#18847,#18848,#18849,#18850,
#18851,#18852,#18853,#18854,#18855,#18856,#18857,#18858,#18859,#18860,#18861,
#18862,#18863,#18864,#18865,#18866,#18867,#18868,#18869,#18870,#18871,#18872,
#18873,#18874,#18875,#18876,#18877,#18878,#18879,#18880,#18881,#18882,#18883,
#18884,#18885));
#19560=CLOSED_SHELL('',(#18886,#18887,#18888,#18889,#18890,#18891));
#19561=CLOSED_SHELL('',(#18892,#18893,#18894,#18895,#18896,#18897,#18898,
#18899,#18900));
#19562=CLOSED_SHELL('',(#18901,#18902,#18903,#18904,#18905,#18906,#18907,
#18908,#18909));
#19563=CLOSED_SHELL('',(#18910,#18911,#18912,#18913,#18914,#18915,#18916,
#18917,#18918,#18919,#18920,#18921,#18922,#18923,#18924,#18925,#18926,#18927,
#18928,#18929,#18930,#18931));
#19564=CLOSED_SHELL('',(#18932,#18933,#18934,#18935,#18936,#18937,#18938,
#18939,#18940,#18941,#18942,#18943,#18944,#18945,#18946,#18947,#18948,#18949,
#18950,#18951,#18952,#18953,#18954,#18955,#18956,#18957,#18958,#18959,#18960,
#18961,#18962,#18963,#18964,#18965,#18966,#18967));
#19565=CLOSED_SHELL('',(#18968,#18969,#18970,#18971,#18972,#18973,#18974,
#18975,#18976,#18977,#18978,#18979,#18980,#18981,#18982,#18983,#18984,#18985,
#18986,#18987,#18988,#18989,#18990,#18991,#18992,#18993,#18994,#18995,#18996,
#18997,#18998,#18999,#19000,#19001,#19002,#19003,#19004,#19005,#19006,#19007,
#19008,#19009,#19010,#19011,#19012,#19013,#19014,#19015,#19016,#19017,#19018,
#19019,#19020,#19021,#19022,#19023,#19024));
#19566=CLOSED_SHELL('',(#19025,#19026,#19027,#19028,#19029,#19030,#19031,
#19032,#19033,#19034,#19035,#19036,#19037,#19038,#19039,#19040,#19041,#19042,
#19043,#19044,#19045,#19046,#19047,#19048,#19049,#19050,#19051,#19052,#19053,
#19054,#19055,#19056,#19057,#19058,#19059,#19060));
#19567=CLOSED_SHELL('',(#19061,#19062,#19063,#19064,#19065,#19066,#19067,
#19068,#19069,#19070,#19071,#19072));
#19568=CLOSED_SHELL('',(#19073,#19074,#19075,#19076,#19077,#19078,#19079,
#19080,#19081,#19082,#19083,#19084,#19085,#19086,#19087,#19088));
#19569=CLOSED_SHELL('',(#19089,#19090,#19091,#19092,#19093,#19094,#19095,
#19096,#19097,#19098,#19099,#19100,#19101,#19102,#19103,#19104,#19105,#19106,
#19107,#19108,#19109,#19110));
#19570=CLOSED_SHELL('',(#19111,#19112,#19113,#19114,#19115,#19116,#19117,
#19118,#19119));
#19571=CLOSED_SHELL('',(#19120,#19121,#19122,#19123,#19124,#19125,#19126,
#19127,#19128,#19129,#19130,#19131,#19132,#19133,#19134,#19135,#19136,#19137,
#19138,#19139,#19140,#19141,#19142,#19143,#19144,#19145,#19146,#19147,#19148,
#19149,#19150,#19151,#19152,#19153,#19154,#19155));
#19572=CLOSED_SHELL('',(#19156,#19157,#19158,#19159));
#19573=CLOSED_SHELL('',(#19160,#19161,#19162,#19163,#19164,#19165,#19166,
#19167,#19168));
#19574=CLOSED_SHELL('',(#19169,#19170,#19171,#19172,#19173,#19174,#19175,
#19176,#19177,#19178,#19179,#19180,#19181,#19182,#19183,#19184,#19185,#19186,
#19187,#19188,#19189,#19190,#19191,#19192,#19193,#19194,#19195,#19196,#19197,
#19198,#19199,#19200,#19201,#19202,#19203,#19204,#19205,#19206,#19207,#19208,
#19209,#19210,#19211,#19212,#19213,#19214,#19215,#19216,#19217,#19218,#19219,
#19220,#19221,#19222,#19223,#19224,#19225,#19226,#19227,#19228,#19229,#19230,
#19231,#19232,#19233,#19234,#19235,#19236,#19237,#19238,#19239,#19240,#19241,
#19242,#19243,#19244,#19245,#19246,#19247,#19248,#19249,#19250,#19251,#19252,
#19253,#19254,#19255,#19256,#19257,#19258,#19259,#19260,#19261));
#19575=CLOSED_SHELL('',(#19262,#19263,#19264,#19265,#19266,#19267));
#19576=CLOSED_SHELL('',(#19268,#19269,#19270,#19271,#19272,#19273,#19274,
#19275,#19276,#19277,#19278,#19279,#19280,#19281,#19282,#19283,#19284,#19285,
#19286,#19287,#19288,#19289,#19290,#19291,#19292,#19293,#19294,#19295,#19296,
#19297,#19298,#19299,#19300,#19301,#19302,#19303));
#19577=CLOSED_SHELL('',(#19304,#19305,#19306,#19307,#19308,#19309,#19310,
#19311,#19312));
#19578=CLOSED_SHELL('',(#19313,#19314,#19315,#19316,#19317,#19318,#19319,
#19320,#19321,#19322,#19323,#19324,#19325,#19326,#19327,#19328,#19329,#19330,
#19331,#19332,#19333,#19334,#19335,#19336,#19337,#19338,#19339,#19340,#19341,
#19342));
#19579=CLOSED_SHELL('',(#19343,#19344,#19345,#19346,#19347,#19348,#19349,
#19350,#19351,#19352,#19353,#19354,#19355,#19356,#19357,#19358,#19359,#19360,
#19361,#19362,#19363,#19364,#19365,#19366,#19367,#19368,#19369,#19370,#19371,
#19372,#19373,#19374,#19375,#19376,#19377,#19378));
#19580=CLOSED_SHELL('',(#19379,#19380,#19381,#19382,#19383,#19384,#19385,
#19386,#19387,#19388,#19389,#19390,#19391,#19392,#19393,#19394,#19395,#19396,
#19397,#19398,#19399,#19400,#19401,#19402,#19403,#19404,#19405,#19406,#19407,
#19408,#19409,#19410,#19411,#19412,#19413,#19414,#19415,#19416,#19417,#19418,
#19419,#19420,#19421,#19422,#19423,#19424,#19425,#19426,#19427,#19428,#19429,
#19430,#19431,#19432));
#19581=CLOSED_SHELL('',(#19433,#19434,#19435,#19436));
#19582=CLOSED_SHELL('',(#19437,#19438,#19439,#19440,#19441,#19442,#19443,
#19444,#19445,#19446,#19447,#19448,#19449,#19450,#19451,#19452,#19453,#19454,
#19455,#19456,#19457,#19458,#19459,#19460,#19461,#19462,#19463,#19464,#19465,
#19466,#19467,#19468,#19469,#19470,#19471,#19472));
#19583=CLOSED_SHELL('',(#19473,#19474,#19475,#19476,#19477,#19478,#19479,
#19480,#19481,#19482,#19483,#19484,#19485,#19486,#19487,#19488,#19489,#19490,
#19491,#19492,#19493,#19494,#19495,#19496,#19497,#19498,#19499,#19500,#19501,
#19502,#19503,#19504,#19505,#19506,#19507,#19508));
#19584=CLOSED_SHELL('',(#19509,#19510,#19511,#19512,#19513,#19514));
#19585=CLOSED_SHELL('',(#19515,#19516,#19517,#19518,#19519,#19520,#19521,
#19522,#19523));
#19586=CLOSED_SHELL('',(#19524,#19525,#19526,#19527,#19528,#19529,#19530,
#19531,#19532,#19533,#19534,#19535,#19536,#19537,#19538,#19539,#19540,#19541,
#19542,#19543,#19544,#19545,#19546,#19547,#19548,#19549,#19550,#19551,#19552,
#19553));
#19587=DERIVED_UNIT_ELEMENT(#19653,1.);
#19588=DERIVED_UNIT_ELEMENT(#34877,-3.);
#19589=DERIVED_UNIT_ELEMENT(#19653,1.);
#19590=DERIVED_UNIT_ELEMENT(#34877,-3.);
#19591=DERIVED_UNIT_ELEMENT(#19653,1.);
#19592=DERIVED_UNIT_ELEMENT(#34877,-3.);
#19593=DERIVED_UNIT_ELEMENT(#19653,1.);
#19594=DERIVED_UNIT_ELEMENT(#34877,-3.);
#19595=DERIVED_UNIT_ELEMENT(#19653,1.);
#19596=DERIVED_UNIT_ELEMENT(#34877,-3.);
#19597=DERIVED_UNIT_ELEMENT(#19653,1.);
#19598=DERIVED_UNIT_ELEMENT(#34877,-3.);
#19599=DERIVED_UNIT_ELEMENT(#19653,1.);
#19600=DERIVED_UNIT_ELEMENT(#34877,-3.);
#19601=DERIVED_UNIT_ELEMENT(#19653,1.);
#19602=DERIVED_UNIT_ELEMENT(#34877,-3.);
#19603=DERIVED_UNIT_ELEMENT(#19653,1.);
#19604=DERIVED_UNIT_ELEMENT(#34877,-3.);
#19605=DERIVED_UNIT_ELEMENT(#19653,1.);
#19606=DERIVED_UNIT_ELEMENT(#34877,-3.);
#19607=DERIVED_UNIT_ELEMENT(#19653,1.);
#19608=DERIVED_UNIT_ELEMENT(#34877,-3.);
#19609=DERIVED_UNIT_ELEMENT(#19653,1.);
#19610=DERIVED_UNIT_ELEMENT(#34877,-3.);
#19611=DERIVED_UNIT_ELEMENT(#19653,1.);
#19612=DERIVED_UNIT_ELEMENT(#34877,-3.);
#19613=DERIVED_UNIT_ELEMENT(#19653,1.);
#19614=DERIVED_UNIT_ELEMENT(#34877,-3.);
#19615=DERIVED_UNIT_ELEMENT(#19653,1.);
#19616=DERIVED_UNIT_ELEMENT(#34877,-3.);
#19617=DERIVED_UNIT_ELEMENT(#19653,1.);
#19618=DERIVED_UNIT_ELEMENT(#34877,-3.);
#19619=DERIVED_UNIT_ELEMENT(#19653,1.);
#19620=DERIVED_UNIT_ELEMENT(#34877,-3.);
#19621=DERIVED_UNIT_ELEMENT(#19653,1.);
#19622=DERIVED_UNIT_ELEMENT(#34877,-3.);
#19623=DERIVED_UNIT_ELEMENT(#19653,1.);
#19624=DERIVED_UNIT_ELEMENT(#34877,-3.);
#19625=DERIVED_UNIT_ELEMENT(#19653,1.);
#19626=DERIVED_UNIT_ELEMENT(#34877,-3.);
#19627=DERIVED_UNIT_ELEMENT(#19653,1.);
#19628=DERIVED_UNIT_ELEMENT(#34877,-3.);
#19629=DERIVED_UNIT_ELEMENT(#19653,1.);
#19630=DERIVED_UNIT_ELEMENT(#34877,-3.);
#19631=DERIVED_UNIT_ELEMENT(#19653,1.);
#19632=DERIVED_UNIT_ELEMENT(#34877,-3.);
#19633=DERIVED_UNIT_ELEMENT(#19653,1.);
#19634=DERIVED_UNIT_ELEMENT(#34877,-3.);
#19635=DERIVED_UNIT_ELEMENT(#19653,1.);
#19636=DERIVED_UNIT_ELEMENT(#34877,-3.);
#19637=DERIVED_UNIT_ELEMENT(#19653,1.);
#19638=DERIVED_UNIT_ELEMENT(#34877,-3.);
#19639=DERIVED_UNIT_ELEMENT(#19653,1.);
#19640=DERIVED_UNIT_ELEMENT(#34877,-3.);
#19641=DERIVED_UNIT_ELEMENT(#19653,1.);
#19642=DERIVED_UNIT_ELEMENT(#34877,-3.);
#19643=DERIVED_UNIT_ELEMENT(#19653,1.);
#19644=DERIVED_UNIT_ELEMENT(#34877,-3.);
#19645=DERIVED_UNIT_ELEMENT(#19653,1.);
#19646=DERIVED_UNIT_ELEMENT(#34877,-3.);
#19647=DERIVED_UNIT_ELEMENT(#19653,1.);
#19648=DERIVED_UNIT_ELEMENT(#34877,-3.);
#19649=DERIVED_UNIT_ELEMENT(#19653,1.);
#19650=DERIVED_UNIT_ELEMENT(#34877,-3.);
#19651=DERIVED_UNIT_ELEMENT(#19653,1.);
#19652=DERIVED_UNIT_ELEMENT(#34877,-3.);
#19653=(
MASS_UNIT()
NAMED_UNIT(*)
SI_UNIT(.KILO.,.GRAM.)
);
#19654=DERIVED_UNIT((#19587,#19588));
#19655=DERIVED_UNIT((#19589,#19590));
#19656=DERIVED_UNIT((#19591,#19592));
#19657=DERIVED_UNIT((#19593,#19594));
#19658=DERIVED_UNIT((#19595,#19596));
#19659=DERIVED_UNIT((#19597,#19598));
#19660=DERIVED_UNIT((#19599,#19600));
#19661=DERIVED_UNIT((#19601,#19602));
#19662=DERIVED_UNIT((#19603,#19604));
#19663=DERIVED_UNIT((#19605,#19606));
#19664=DERIVED_UNIT((#19607,#19608));
#19665=DERIVED_UNIT((#19609,#19610));
#19666=DERIVED_UNIT((#19611,#19612));
#19667=DERIVED_UNIT((#19613,#19614));
#19668=DERIVED_UNIT((#19615,#19616));
#19669=DERIVED_UNIT((#19617,#19618));
#19670=DERIVED_UNIT((#19619,#19620));
#19671=DERIVED_UNIT((#19621,#19622));
#19672=DERIVED_UNIT((#19623,#19624));
#19673=DERIVED_UNIT((#19625,#19626));
#19674=DERIVED_UNIT((#19627,#19628));
#19675=DERIVED_UNIT((#19629,#19630));
#19676=DERIVED_UNIT((#19631,#19632));
#19677=DERIVED_UNIT((#19633,#19634));
#19678=DERIVED_UNIT((#19635,#19636));
#19679=DERIVED_UNIT((#19637,#19638));
#19680=DERIVED_UNIT((#19639,#19640));
#19681=DERIVED_UNIT((#19641,#19642));
#19682=DERIVED_UNIT((#19643,#19644));
#19683=DERIVED_UNIT((#19645,#19646));
#19684=DERIVED_UNIT((#19647,#19648));
#19685=DERIVED_UNIT((#19649,#19650));
#19686=DERIVED_UNIT((#19651,#19652));
#19687=MEASURE_REPRESENTATION_ITEM('density measure',
POSITIVE_RATIO_MEASURE(7850.),#19654);
#19688=MEASURE_REPRESENTATION_ITEM('density measure',
POSITIVE_RATIO_MEASURE(7850.),#19655);
#19689=MEASURE_REPRESENTATION_ITEM('density measure',
POSITIVE_RATIO_MEASURE(7850.),#19656);
#19690=MEASURE_REPRESENTATION_ITEM('density measure',
POSITIVE_RATIO_MEASURE(7850.),#19657);
#19691=MEASURE_REPRESENTATION_ITEM('density measure',
POSITIVE_RATIO_MEASURE(7850.),#19658);
#19692=MEASURE_REPRESENTATION_ITEM('density measure',
POSITIVE_RATIO_MEASURE(7850.),#19659);
#19693=MEASURE_REPRESENTATION_ITEM('density measure',
POSITIVE_RATIO_MEASURE(7850.),#19660);
#19694=MEASURE_REPRESENTATION_ITEM('density measure',
POSITIVE_RATIO_MEASURE(7850.),#19661);
#19695=MEASURE_REPRESENTATION_ITEM('density measure',
POSITIVE_RATIO_MEASURE(7850.),#19662);
#19696=MEASURE_REPRESENTATION_ITEM('density measure',
POSITIVE_RATIO_MEASURE(7850.),#19663);
#19697=MEASURE_REPRESENTATION_ITEM('density measure',
POSITIVE_RATIO_MEASURE(7850.),#19664);
#19698=MEASURE_REPRESENTATION_ITEM('density measure',
POSITIVE_RATIO_MEASURE(7850.),#19665);
#19699=MEASURE_REPRESENTATION_ITEM('density measure',
POSITIVE_RATIO_MEASURE(7850.),#19666);
#19700=MEASURE_REPRESENTATION_ITEM('density measure',
POSITIVE_RATIO_MEASURE(7850.),#19667);
#19701=MEASURE_REPRESENTATION_ITEM('density measure',
POSITIVE_RATIO_MEASURE(7850.),#19668);
#19702=MEASURE_REPRESENTATION_ITEM('density measure',
POSITIVE_RATIO_MEASURE(7850.),#19669);
#19703=MEASURE_REPRESENTATION_ITEM('density measure',
POSITIVE_RATIO_MEASURE(7850.),#19670);
#19704=MEASURE_REPRESENTATION_ITEM('density measure',
POSITIVE_RATIO_MEASURE(7850.),#19671);
#19705=MEASURE_REPRESENTATION_ITEM('density measure',
POSITIVE_RATIO_MEASURE(7850.),#19672);
#19706=MEASURE_REPRESENTATION_ITEM('density measure',
POSITIVE_RATIO_MEASURE(7850.),#19673);
#19707=MEASURE_REPRESENTATION_ITEM('density measure',
POSITIVE_RATIO_MEASURE(7850.),#19674);
#19708=MEASURE_REPRESENTATION_ITEM('density measure',
POSITIVE_RATIO_MEASURE(7850.),#19675);
#19709=MEASURE_REPRESENTATION_ITEM('density measure',
POSITIVE_RATIO_MEASURE(7850.),#19676);
#19710=MEASURE_REPRESENTATION_ITEM('density measure',
POSITIVE_RATIO_MEASURE(7850.),#19677);
#19711=MEASURE_REPRESENTATION_ITEM('density measure',
POSITIVE_RATIO_MEASURE(7850.),#19678);
#19712=MEASURE_REPRESENTATION_ITEM('density measure',
POSITIVE_RATIO_MEASURE(7850.),#19679);
#19713=MEASURE_REPRESENTATION_ITEM('density measure',
POSITIVE_RATIO_MEASURE(7850.),#19680);
#19714=MEASURE_REPRESENTATION_ITEM('density measure',
POSITIVE_RATIO_MEASURE(7850.),#19681);
#19715=MEASURE_REPRESENTATION_ITEM('density measure',
POSITIVE_RATIO_MEASURE(7850.),#19682);
#19716=MEASURE_REPRESENTATION_ITEM('density measure',
POSITIVE_RATIO_MEASURE(7850.),#19683);
#19717=MEASURE_REPRESENTATION_ITEM('density measure',
POSITIVE_RATIO_MEASURE(7850.),#19684);
#19718=MEASURE_REPRESENTATION_ITEM('density measure',
POSITIVE_RATIO_MEASURE(7850.),#19685);
#19719=MEASURE_REPRESENTATION_ITEM('density measure',
POSITIVE_RATIO_MEASURE(7850.),#19686);
#19720=PROPERTY_DEFINITION_REPRESENTATION(#19885,#19786);
#19721=PROPERTY_DEFINITION_REPRESENTATION(#19886,#19787);
#19722=PROPERTY_DEFINITION_REPRESENTATION(#19887,#19788);
#19723=PROPERTY_DEFINITION_REPRESENTATION(#19888,#19789);
#19724=PROPERTY_DEFINITION_REPRESENTATION(#19889,#19790);
#19725=PROPERTY_DEFINITION_REPRESENTATION(#19890,#19791);
#19726=PROPERTY_DEFINITION_REPRESENTATION(#19891,#19792);
#19727=PROPERTY_DEFINITION_REPRESENTATION(#19892,#19793);
#19728=PROPERTY_DEFINITION_REPRESENTATION(#19893,#19794);
#19729=PROPERTY_DEFINITION_REPRESENTATION(#19894,#19795);
#19730=PROPERTY_DEFINITION_REPRESENTATION(#19895,#19796);
#19731=PROPERTY_DEFINITION_REPRESENTATION(#19896,#19797);
#19732=PROPERTY_DEFINITION_REPRESENTATION(#19897,#19798);
#19733=PROPERTY_DEFINITION_REPRESENTATION(#19898,#19799);
#19734=PROPERTY_DEFINITION_REPRESENTATION(#19899,#19800);
#19735=PROPERTY_DEFINITION_REPRESENTATION(#19900,#19801);
#19736=PROPERTY_DEFINITION_REPRESENTATION(#19901,#19802);
#19737=PROPERTY_DEFINITION_REPRESENTATION(#19902,#19803);
#19738=PROPERTY_DEFINITION_REPRESENTATION(#19903,#19804);
#19739=PROPERTY_DEFINITION_REPRESENTATION(#19904,#19805);
#19740=PROPERTY_DEFINITION_REPRESENTATION(#19905,#19806);
#19741=PROPERTY_DEFINITION_REPRESENTATION(#19906,#19807);
#19742=PROPERTY_DEFINITION_REPRESENTATION(#19907,#19808);
#19743=PROPERTY_DEFINITION_REPRESENTATION(#19908,#19809);
#19744=PROPERTY_DEFINITION_REPRESENTATION(#19909,#19810);
#19745=PROPERTY_DEFINITION_REPRESENTATION(#19910,#19811);
#19746=PROPERTY_DEFINITION_REPRESENTATION(#19911,#19812);
#19747=PROPERTY_DEFINITION_REPRESENTATION(#19912,#19813);
#19748=PROPERTY_DEFINITION_REPRESENTATION(#19913,#19814);
#19749=PROPERTY_DEFINITION_REPRESENTATION(#19914,#19815);
#19750=PROPERTY_DEFINITION_REPRESENTATION(#19915,#19816);
#19751=PROPERTY_DEFINITION_REPRESENTATION(#19916,#19817);
#19752=PROPERTY_DEFINITION_REPRESENTATION(#19917,#19818);
#19753=PROPERTY_DEFINITION_REPRESENTATION(#19918,#19819);
#19754=PROPERTY_DEFINITION_REPRESENTATION(#19919,#19820);
#19755=PROPERTY_DEFINITION_REPRESENTATION(#19920,#19821);
#19756=PROPERTY_DEFINITION_REPRESENTATION(#19921,#19822);
#19757=PROPERTY_DEFINITION_REPRESENTATION(#19922,#19823);
#19758=PROPERTY_DEFINITION_REPRESENTATION(#19923,#19824);
#19759=PROPERTY_DEFINITION_REPRESENTATION(#19924,#19825);
#19760=PROPERTY_DEFINITION_REPRESENTATION(#19925,#19826);
#19761=PROPERTY_DEFINITION_REPRESENTATION(#19926,#19827);
#19762=PROPERTY_DEFINITION_REPRESENTATION(#19927,#19828);
#19763=PROPERTY_DEFINITION_REPRESENTATION(#19928,#19829);
#19764=PROPERTY_DEFINITION_REPRESENTATION(#19929,#19830);
#19765=PROPERTY_DEFINITION_REPRESENTATION(#19930,#19831);
#19766=PROPERTY_DEFINITION_REPRESENTATION(#19931,#19832);
#19767=PROPERTY_DEFINITION_REPRESENTATION(#19932,#19833);
#19768=PROPERTY_DEFINITION_REPRESENTATION(#19933,#19834);
#19769=PROPERTY_DEFINITION_REPRESENTATION(#19934,#19835);
#19770=PROPERTY_DEFINITION_REPRESENTATION(#19935,#19836);
#19771=PROPERTY_DEFINITION_REPRESENTATION(#19936,#19837);
#19772=PROPERTY_DEFINITION_REPRESENTATION(#19937,#19838);
#19773=PROPERTY_DEFINITION_REPRESENTATION(#19938,#19839);
#19774=PROPERTY_DEFINITION_REPRESENTATION(#19939,#19840);
#19775=PROPERTY_DEFINITION_REPRESENTATION(#19940,#19841);
#19776=PROPERTY_DEFINITION_REPRESENTATION(#19941,#19842);
#19777=PROPERTY_DEFINITION_REPRESENTATION(#19942,#19843);
#19778=PROPERTY_DEFINITION_REPRESENTATION(#19943,#19844);
#19779=PROPERTY_DEFINITION_REPRESENTATION(#19944,#19845);
#19780=PROPERTY_DEFINITION_REPRESENTATION(#19945,#19846);
#19781=PROPERTY_DEFINITION_REPRESENTATION(#19946,#19847);
#19782=PROPERTY_DEFINITION_REPRESENTATION(#19947,#19848);
#19783=PROPERTY_DEFINITION_REPRESENTATION(#19948,#19849);
#19784=PROPERTY_DEFINITION_REPRESENTATION(#19949,#19850);
#19785=PROPERTY_DEFINITION_REPRESENTATION(#19950,#19851);
#19786=REPRESENTATION('material name',(#19852),#34843);
#19787=REPRESENTATION('density',(#19687),#34843);
#19788=REPRESENTATION('material name',(#19853),#34844);
#19789=REPRESENTATION('density',(#19688),#34844);
#19790=REPRESENTATION('material name',(#19854),#34845);
#19791=REPRESENTATION('density',(#19689),#34845);
#19792=REPRESENTATION('material name',(#19855),#34846);
#19793=REPRESENTATION('density',(#19690),#34846);
#19794=REPRESENTATION('material name',(#19856),#34847);
#19795=REPRESENTATION('density',(#19691),#34847);
#19796=REPRESENTATION('material name',(#19857),#34848);
#19797=REPRESENTATION('density',(#19692),#34848);
#19798=REPRESENTATION('material name',(#19858),#34849);
#19799=REPRESENTATION('density',(#19693),#34849);
#19800=REPRESENTATION('material name',(#19859),#34850);
#19801=REPRESENTATION('density',(#19694),#34850);
#19802=REPRESENTATION('material name',(#19860),#34851);
#19803=REPRESENTATION('density',(#19695),#34851);
#19804=REPRESENTATION('material name',(#19861),#34852);
#19805=REPRESENTATION('density',(#19696),#34852);
#19806=REPRESENTATION('material name',(#19862),#34853);
#19807=REPRESENTATION('density',(#19697),#34853);
#19808=REPRESENTATION('material name',(#19863),#34854);
#19809=REPRESENTATION('density',(#19698),#34854);
#19810=REPRESENTATION('material name',(#19864),#34855);
#19811=REPRESENTATION('density',(#19699),#34855);
#19812=REPRESENTATION('material name',(#19865),#34856);
#19813=REPRESENTATION('density',(#19700),#34856);
#19814=REPRESENTATION('material name',(#19866),#34857);
#19815=REPRESENTATION('density',(#19701),#34857);
#19816=REPRESENTATION('material name',(#19867),#34858);
#19817=REPRESENTATION('density',(#19702),#34858);
#19818=REPRESENTATION('material name',(#19868),#34859);
#19819=REPRESENTATION('density',(#19703),#34859);
#19820=REPRESENTATION('material name',(#19869),#34860);
#19821=REPRESENTATION('density',(#19704),#34860);
#19822=REPRESENTATION('material name',(#19870),#34861);
#19823=REPRESENTATION('density',(#19705),#34861);
#19824=REPRESENTATION('material name',(#19871),#34862);
#19825=REPRESENTATION('density',(#19706),#34862);
#19826=REPRESENTATION('material name',(#19872),#34863);
#19827=REPRESENTATION('density',(#19707),#34863);
#19828=REPRESENTATION('material name',(#19873),#34864);
#19829=REPRESENTATION('density',(#19708),#34864);
#19830=REPRESENTATION('material name',(#19874),#34865);
#19831=REPRESENTATION('density',(#19709),#34865);
#19832=REPRESENTATION('material name',(#19875),#34866);
#19833=REPRESENTATION('density',(#19710),#34866);
#19834=REPRESENTATION('material name',(#19876),#34867);
#19835=REPRESENTATION('density',(#19711),#34867);
#19836=REPRESENTATION('material name',(#19877),#34868);
#19837=REPRESENTATION('density',(#19712),#34868);
#19838=REPRESENTATION('material name',(#19878),#34869);
#19839=REPRESENTATION('density',(#19713),#34869);
#19840=REPRESENTATION('material name',(#19879),#34870);
#19841=REPRESENTATION('density',(#19714),#34870);
#19842=REPRESENTATION('material name',(#19880),#34871);
#19843=REPRESENTATION('density',(#19715),#34871);
#19844=REPRESENTATION('material name',(#19881),#34872);
#19845=REPRESENTATION('density',(#19716),#34872);
#19846=REPRESENTATION('material name',(#19882),#34873);
#19847=REPRESENTATION('density',(#19717),#34873);
#19848=REPRESENTATION('material name',(#19883),#34874);
#19849=REPRESENTATION('density',(#19718),#34874);
#19850=REPRESENTATION('material name',(#19884),#34875);
#19851=REPRESENTATION('density',(#19719),#34875);
#19852=DESCRIPTIVE_REPRESENTATION_ITEM('Steel','Steel');
#19853=DESCRIPTIVE_REPRESENTATION_ITEM('Steel','Steel');
#19854=DESCRIPTIVE_REPRESENTATION_ITEM('Steel','Steel');
#19855=DESCRIPTIVE_REPRESENTATION_ITEM('Steel','Steel');
#19856=DESCRIPTIVE_REPRESENTATION_ITEM('Steel','Steel');
#19857=DESCRIPTIVE_REPRESENTATION_ITEM('Steel','Steel');
#19858=DESCRIPTIVE_REPRESENTATION_ITEM('Steel','Steel');
#19859=DESCRIPTIVE_REPRESENTATION_ITEM('Steel','Steel');
#19860=DESCRIPTIVE_REPRESENTATION_ITEM('Steel','Steel');
#19861=DESCRIPTIVE_REPRESENTATION_ITEM('Steel','Steel');
#19862=DESCRIPTIVE_REPRESENTATION_ITEM('Steel','Steel');
#19863=DESCRIPTIVE_REPRESENTATION_ITEM('Steel','Steel');
#19864=DESCRIPTIVE_REPRESENTATION_ITEM('Steel','Steel');
#19865=DESCRIPTIVE_REPRESENTATION_ITEM('Steel','Steel');
#19866=DESCRIPTIVE_REPRESENTATION_ITEM('Steel','Steel');
#19867=DESCRIPTIVE_REPRESENTATION_ITEM('Steel','Steel');
#19868=DESCRIPTIVE_REPRESENTATION_ITEM('Steel','Steel');
#19869=DESCRIPTIVE_REPRESENTATION_ITEM('Steel','Steel');
#19870=DESCRIPTIVE_REPRESENTATION_ITEM('Steel','Steel');
#19871=DESCRIPTIVE_REPRESENTATION_ITEM('Steel','Steel');
#19872=DESCRIPTIVE_REPRESENTATION_ITEM('Steel','Steel');
#19873=DESCRIPTIVE_REPRESENTATION_ITEM('Steel','Steel');
#19874=DESCRIPTIVE_REPRESENTATION_ITEM('Steel','Steel');
#19875=DESCRIPTIVE_REPRESENTATION_ITEM('Steel','Steel');
#19876=DESCRIPTIVE_REPRESENTATION_ITEM('Steel','Steel');
#19877=DESCRIPTIVE_REPRESENTATION_ITEM('Steel','Steel');
#19878=DESCRIPTIVE_REPRESENTATION_ITEM('Steel','Steel');
#19879=DESCRIPTIVE_REPRESENTATION_ITEM('Steel','Steel');
#19880=DESCRIPTIVE_REPRESENTATION_ITEM('Steel','Steel');
#19881=DESCRIPTIVE_REPRESENTATION_ITEM('Steel','Steel');
#19882=DESCRIPTIVE_REPRESENTATION_ITEM('Steel','Steel');
#19883=DESCRIPTIVE_REPRESENTATION_ITEM('Steel','Steel');
#19884=DESCRIPTIVE_REPRESENTATION_ITEM('Steel','Steel');
#19885=PROPERTY_DEFINITION('material property','material name',#35020);
#19886=PROPERTY_DEFINITION('material property','density of part',#35020);
#19887=PROPERTY_DEFINITION('material property','material name',#35021);
#19888=PROPERTY_DEFINITION('material property','density of part',#35021);
#19889=PROPERTY_DEFINITION('material property','material name',#35022);
#19890=PROPERTY_DEFINITION('material property','density of part',#35022);
#19891=PROPERTY_DEFINITION('material property','material name',#35023);
#19892=PROPERTY_DEFINITION('material property','density of part',#35023);
#19893=PROPERTY_DEFINITION('material property','material name',#35024);
#19894=PROPERTY_DEFINITION('material property','density of part',#35024);
#19895=PROPERTY_DEFINITION('material property','material name',#35025);
#19896=PROPERTY_DEFINITION('material property','density of part',#35025);
#19897=PROPERTY_DEFINITION('material property','material name',#35026);
#19898=PROPERTY_DEFINITION('material property','density of part',#35026);
#19899=PROPERTY_DEFINITION('material property','material name',#35027);
#19900=PROPERTY_DEFINITION('material property','density of part',#35027);
#19901=PROPERTY_DEFINITION('material property','material name',#35028);
#19902=PROPERTY_DEFINITION('material property','density of part',#35028);
#19903=PROPERTY_DEFINITION('material property','material name',#35029);
#19904=PROPERTY_DEFINITION('material property','density of part',#35029);
#19905=PROPERTY_DEFINITION('material property','material name',#35030);
#19906=PROPERTY_DEFINITION('material property','density of part',#35030);
#19907=PROPERTY_DEFINITION('material property','material name',#35031);
#19908=PROPERTY_DEFINITION('material property','density of part',#35031);
#19909=PROPERTY_DEFINITION('material property','material name',#35032);
#19910=PROPERTY_DEFINITION('material property','density of part',#35032);
#19911=PROPERTY_DEFINITION('material property','material name',#35033);
#19912=PROPERTY_DEFINITION('material property','density of part',#35033);
#19913=PROPERTY_DEFINITION('material property','material name',#35034);
#19914=PROPERTY_DEFINITION('material property','density of part',#35034);
#19915=PROPERTY_DEFINITION('material property','material name',#35035);
#19916=PROPERTY_DEFINITION('material property','density of part',#35035);
#19917=PROPERTY_DEFINITION('material property','material name',#35036);
#19918=PROPERTY_DEFINITION('material property','density of part',#35036);
#19919=PROPERTY_DEFINITION('material property','material name',#35037);
#19920=PROPERTY_DEFINITION('material property','density of part',#35037);
#19921=PROPERTY_DEFINITION('material property','material name',#35038);
#19922=PROPERTY_DEFINITION('material property','density of part',#35038);
#19923=PROPERTY_DEFINITION('material property','material name',#35039);
#19924=PROPERTY_DEFINITION('material property','density of part',#35039);
#19925=PROPERTY_DEFINITION('material property','material name',#35040);
#19926=PROPERTY_DEFINITION('material property','density of part',#35040);
#19927=PROPERTY_DEFINITION('material property','material name',#35041);
#19928=PROPERTY_DEFINITION('material property','density of part',#35041);
#19929=PROPERTY_DEFINITION('material property','material name',#35042);
#19930=PROPERTY_DEFINITION('material property','density of part',#35042);
#19931=PROPERTY_DEFINITION('material property','material name',#35043);
#19932=PROPERTY_DEFINITION('material property','density of part',#35043);
#19933=PROPERTY_DEFINITION('material property','material name',#35044);
#19934=PROPERTY_DEFINITION('material property','density of part',#35044);
#19935=PROPERTY_DEFINITION('material property','material name',#35045);
#19936=PROPERTY_DEFINITION('material property','density of part',#35045);
#19937=PROPERTY_DEFINITION('material property','material name',#35046);
#19938=PROPERTY_DEFINITION('material property','density of part',#35046);
#19939=PROPERTY_DEFINITION('material property','material name',#35047);
#19940=PROPERTY_DEFINITION('material property','density of part',#35047);
#19941=PROPERTY_DEFINITION('material property','material name',#35048);
#19942=PROPERTY_DEFINITION('material property','density of part',#35048);
#19943=PROPERTY_DEFINITION('material property','material name',#35049);
#19944=PROPERTY_DEFINITION('material property','density of part',#35049);
#19945=PROPERTY_DEFINITION('material property','material name',#35050);
#19946=PROPERTY_DEFINITION('material property','density of part',#35050);
#19947=PROPERTY_DEFINITION('material property','material name',#35051);
#19948=PROPERTY_DEFINITION('material property','density of part',#35051);
#19949=PROPERTY_DEFINITION('material property','material name',#35052);
#19950=PROPERTY_DEFINITION('material property','density of part',#35052);
#19951=AXIS2_PLACEMENT_3D('',#28471,#22258,#22259);
#19952=AXIS2_PLACEMENT_3D('',#28472,#22260,#22261);
#19953=AXIS2_PLACEMENT_3D('',#28473,#22262,#22263);
#19954=AXIS2_PLACEMENT_3D('',#28475,#22264,#22265);
#19955=AXIS2_PLACEMENT_3D('',#28477,#22266,#22267);
#19956=AXIS2_PLACEMENT_3D('',#28479,#22268,#22269);
#19957=AXIS2_PLACEMENT_3D('',#28480,#22270,#22271);
#19958=AXIS2_PLACEMENT_3D('',#28481,#22272,#22273);
#19959=AXIS2_PLACEMENT_3D('',#28485,#22275,#22276);
#19960=AXIS2_PLACEMENT_3D('',#28486,#22277,#22278);
#19961=AXIS2_PLACEMENT_3D('',#28487,#22279,#22280);
#19962=AXIS2_PLACEMENT_3D('',#28489,#22281,#22282);
#19963=AXIS2_PLACEMENT_3D('',#28490,#22283,#22284);
#19964=AXIS2_PLACEMENT_3D('',#28492,#22285,#22286);
#19965=AXIS2_PLACEMENT_3D('',#28493,#22287,#22288);
#19966=AXIS2_PLACEMENT_3D('',#28494,#22289,#22290);
#19967=AXIS2_PLACEMENT_3D('',#28496,#22291,#22292);
#19968=AXIS2_PLACEMENT_3D('',#28497,#22293,#22294);
#19969=AXIS2_PLACEMENT_3D('',#28499,#22296,#22297);
#19970=AXIS2_PLACEMENT_3D('',#28500,#22298,#22299);
#19971=AXIS2_PLACEMENT_3D('',#28503,#22300,#22301);
#19972=AXIS2_PLACEMENT_3D('',#28507,#22303,#22304);
#19973=AXIS2_PLACEMENT_3D('',#28509,#22306,#22307);
#19974=AXIS2_PLACEMENT_3D('',#28511,#22308,#22309);
#19975=AXIS2_PLACEMENT_3D('',#28514,#22311,#22312);
#19976=AXIS2_PLACEMENT_3D('',#28515,#22313,#22314);
#19977=AXIS2_PLACEMENT_3D('',#28517,#22315,#22316);
#19978=AXIS2_PLACEMENT_3D('',#28520,#22318,#22319);
#19979=AXIS2_PLACEMENT_3D('',#28521,#22320,#22321);
#19980=AXIS2_PLACEMENT_3D('',#28527,#22325,#22326);
#19981=AXIS2_PLACEMENT_3D('',#28530,#22327,#22328);
#19982=AXIS2_PLACEMENT_3D('',#28534,#22330,#22331);
#19983=AXIS2_PLACEMENT_3D('',#28536,#22333,#22334);
#19984=AXIS2_PLACEMENT_3D('',#28538,#22335,#22336);
#19985=AXIS2_PLACEMENT_3D('',#28541,#22338,#22339);
#19986=AXIS2_PLACEMENT_3D('',#28542,#22340,#22341);
#19987=AXIS2_PLACEMENT_3D('',#28544,#22342,#22343);
#19988=AXIS2_PLACEMENT_3D('',#28547,#22345,#22346);
#19989=AXIS2_PLACEMENT_3D('',#28548,#22347,#22348);
#19990=AXIS2_PLACEMENT_3D('',#28554,#22352,#22353);
#19991=AXIS2_PLACEMENT_3D('',#28557,#22354,#22355);
#19992=AXIS2_PLACEMENT_3D('',#28561,#22357,#22358);
#19993=AXIS2_PLACEMENT_3D('',#28563,#22360,#22361);
#19994=AXIS2_PLACEMENT_3D('',#28565,#22362,#22363);
#19995=AXIS2_PLACEMENT_3D('',#28568,#22365,#22366);
#19996=AXIS2_PLACEMENT_3D('',#28569,#22367,#22368);
#19997=AXIS2_PLACEMENT_3D('',#28571,#22369,#22370);
#19998=AXIS2_PLACEMENT_3D('',#28574,#22372,#22373);
#19999=AXIS2_PLACEMENT_3D('',#28575,#22374,#22375);
#20000=AXIS2_PLACEMENT_3D('',#28581,#22379,#22380);
#20001=AXIS2_PLACEMENT_3D('',#28584,#22381,#22382);
#20002=AXIS2_PLACEMENT_3D('',#28588,#22384,#22385);
#20003=AXIS2_PLACEMENT_3D('',#28590,#22387,#22388);
#20004=AXIS2_PLACEMENT_3D('',#28592,#22389,#22390);
#20005=AXIS2_PLACEMENT_3D('',#28595,#22392,#22393);
#20006=AXIS2_PLACEMENT_3D('',#28596,#22394,#22395);
#20007=AXIS2_PLACEMENT_3D('',#28598,#22396,#22397);
#20008=AXIS2_PLACEMENT_3D('',#28601,#22399,#22400);
#20009=AXIS2_PLACEMENT_3D('',#28602,#22401,#22402);
#20010=AXIS2_PLACEMENT_3D('',#28608,#22406,#22407);
#20011=AXIS2_PLACEMENT_3D('',#28611,#22408,#22409);
#20012=AXIS2_PLACEMENT_3D('',#28615,#22411,#22412);
#20013=AXIS2_PLACEMENT_3D('',#28617,#22414,#22415);
#20014=AXIS2_PLACEMENT_3D('',#28619,#22416,#22417);
#20015=AXIS2_PLACEMENT_3D('',#28622,#22419,#22420);
#20016=AXIS2_PLACEMENT_3D('',#28623,#22421,#22422);
#20017=AXIS2_PLACEMENT_3D('',#28625,#22423,#22424);
#20018=AXIS2_PLACEMENT_3D('',#28628,#22426,#22427);
#20019=AXIS2_PLACEMENT_3D('',#28629,#22428,#22429);
#20020=AXIS2_PLACEMENT_3D('',#28635,#22433,#22434);
#20021=AXIS2_PLACEMENT_3D('',#28641,#22438,#22439);
#20022=AXIS2_PLACEMENT_3D('',#28647,#22443,#22444);
#20023=AXIS2_PLACEMENT_3D('',#28653,#22448,#22449);
#20024=AXIS2_PLACEMENT_3D('',#28659,#22453,#22454);
#20025=AXIS2_PLACEMENT_3D('',#28661,#22455,#22456);
#20026=AXIS2_PLACEMENT_3D('',#28664,#22458,#22459);
#20027=AXIS2_PLACEMENT_3D('',#28665,#22460,#22461);
#20028=AXIS2_PLACEMENT_3D('',#28666,#22462,#22463);
#20029=AXIS2_PLACEMENT_3D('',#28667,#22464,#22465);
#20030=AXIS2_PLACEMENT_3D('',#28668,#22466,#22467);
#20031=AXIS2_PLACEMENT_3D('',#28672,#22469,#22470);
#20032=AXIS2_PLACEMENT_3D('',#28675,#22472,#22473);
#20033=AXIS2_PLACEMENT_3D('',#28676,#22474,#22475);
#20034=AXIS2_PLACEMENT_3D('',#28678,#22476,#22477);
#20035=AXIS2_PLACEMENT_3D('',#28680,#22479,#22480);
#20036=AXIS2_PLACEMENT_3D('',#28681,#22481,#22482);
#20037=AXIS2_PLACEMENT_3D('',#28683,#22483,#22484);
#20038=AXIS2_PLACEMENT_3D('',#28685,#22486,#22487);
#20039=AXIS2_PLACEMENT_3D('',#28688,#22489,#22490);
#20040=AXIS2_PLACEMENT_3D('',#28689,#22491,#22492);
#20041=AXIS2_PLACEMENT_3D('',#28691,#22494,#22495);
#20042=AXIS2_PLACEMENT_3D('',#28692,#22496,#22497);
#20043=AXIS2_PLACEMENT_3D('',#28693,#22498,#22499);
#20044=AXIS2_PLACEMENT_3D('',#28697,#22501,#22502);
#20045=AXIS2_PLACEMENT_3D('',#28699,#22504,#22505);
#20046=AXIS2_PLACEMENT_3D('',#28701,#22507,#22508);
#20047=AXIS2_PLACEMENT_3D('',#28702,#22509,#22510);
#20048=AXIS2_PLACEMENT_3D('',#28703,#22511,#22512);
#20049=AXIS2_PLACEMENT_3D('',#28705,#22514,#22515);
#20050=AXIS2_PLACEMENT_3D('',#28706,#22516,#22517);
#20051=AXIS2_PLACEMENT_3D('',#28707,#22518,#22519);
#20052=AXIS2_PLACEMENT_3D('',#28709,#22520,#22521);
#20053=AXIS2_PLACEMENT_3D('',#28711,#22522,#22523);
#20054=AXIS2_PLACEMENT_3D('',#28712,#22524,#22525);
#20055=AXIS2_PLACEMENT_3D('',#28715,#22527,#22528);
#20056=AXIS2_PLACEMENT_3D('',#28716,#22529,#22530);
#20057=AXIS2_PLACEMENT_3D('',#28718,#22531,#22532);
#20058=AXIS2_PLACEMENT_3D('',#28720,#22534,#22535);
#20059=AXIS2_PLACEMENT_3D('',#28721,#22536,#22537);
#20060=AXIS2_PLACEMENT_3D('',#28722,#22538,#22539);
#20061=AXIS2_PLACEMENT_3D('',#28725,#22540,#22541);
#20062=AXIS2_PLACEMENT_3D('',#28727,#22542,#22543);
#20063=AXIS2_PLACEMENT_3D('',#28729,#22544,#22545);
#20064=AXIS2_PLACEMENT_3D('',#28733,#22547,#22548);
#20065=AXIS2_PLACEMENT_3D('',#28735,#22549,#22550);
#20066=AXIS2_PLACEMENT_3D('',#28737,#22551,#22552);
#20067=AXIS2_PLACEMENT_3D('',#28781,#22556,#22557);
#20068=AXIS2_PLACEMENT_3D('',#28787,#22561,#22562);
#20069=AXIS2_PLACEMENT_3D('',#28790,#22564,#22565);
#20070=AXIS2_PLACEMENT_3D('',#28791,#22566,#22567);
#20071=AXIS2_PLACEMENT_3D('',#28794,#22569,#22570);
#20072=AXIS2_PLACEMENT_3D('',#28795,#22571,#22572);
#20073=AXIS2_PLACEMENT_3D('',#28797,#22573,#22574);
#20074=AXIS2_PLACEMENT_3D('',#28799,#22576,#22577);
#20075=AXIS2_PLACEMENT_3D('',#28803,#22580,#22581);
#20076=AXIS2_PLACEMENT_3D('',#28806,#22583,#22584);
#20077=AXIS2_PLACEMENT_3D('',#28807,#22585,#22586);
#20078=AXIS2_PLACEMENT_3D('',#28809,#22587,#22588);
#20079=AXIS2_PLACEMENT_3D('',#28810,#22589,#22590);
#20080=AXIS2_PLACEMENT_3D('',#28811,#22591,#22592);
#20081=AXIS2_PLACEMENT_3D('',#28813,#22594,#22595);
#20082=AXIS2_PLACEMENT_3D('',#28814,#22596,#22597);
#20083=AXIS2_PLACEMENT_3D('',#28820,#22601,#22602);
#20084=AXIS2_PLACEMENT_3D('',#28823,#22604,#22605);
#20085=AXIS2_PLACEMENT_3D('',#28824,#22606,#22607);
#20086=AXIS2_PLACEMENT_3D('',#28826,#22608,#22609);
#20087=AXIS2_PLACEMENT_3D('',#28828,#22611,#22612);
#20088=AXIS2_PLACEMENT_3D('',#28830,#22614,#22615);
#20089=AXIS2_PLACEMENT_3D('',#28833,#22616,#22617);
#20090=AXIS2_PLACEMENT_3D('',#28835,#22618,#22619);
#20091=AXIS2_PLACEMENT_3D('',#28837,#22620,#22621);
#20092=AXIS2_PLACEMENT_3D('',#28841,#22623,#22624);
#20093=AXIS2_PLACEMENT_3D('',#28843,#22625,#22626);
#20094=AXIS2_PLACEMENT_3D('',#28845,#22627,#22628);
#20095=AXIS2_PLACEMENT_3D('',#28889,#22632,#22633);
#20096=AXIS2_PLACEMENT_3D('',#28895,#22637,#22638);
#20097=AXIS2_PLACEMENT_3D('',#28898,#22640,#22641);
#20098=AXIS2_PLACEMENT_3D('',#28899,#22642,#22643);
#20099=AXIS2_PLACEMENT_3D('',#28902,#22645,#22646);
#20100=AXIS2_PLACEMENT_3D('',#28903,#22647,#22648);
#20101=AXIS2_PLACEMENT_3D('',#28905,#22649,#22650);
#20102=AXIS2_PLACEMENT_3D('',#28907,#22652,#22653);
#20103=AXIS2_PLACEMENT_3D('',#28911,#22656,#22657);
#20104=AXIS2_PLACEMENT_3D('',#28914,#22659,#22660);
#20105=AXIS2_PLACEMENT_3D('',#28915,#22661,#22662);
#20106=AXIS2_PLACEMENT_3D('',#28917,#22663,#22664);
#20107=AXIS2_PLACEMENT_3D('',#28918,#22665,#22666);
#20108=AXIS2_PLACEMENT_3D('',#28919,#22667,#22668);
#20109=AXIS2_PLACEMENT_3D('',#28921,#22670,#22671);
#20110=AXIS2_PLACEMENT_3D('',#28922,#22672,#22673);
#20111=AXIS2_PLACEMENT_3D('',#28928,#22677,#22678);
#20112=AXIS2_PLACEMENT_3D('',#28931,#22680,#22681);
#20113=AXIS2_PLACEMENT_3D('',#28932,#22682,#22683);
#20114=AXIS2_PLACEMENT_3D('',#28934,#22684,#22685);
#20115=AXIS2_PLACEMENT_3D('',#28936,#22687,#22688);
#20116=AXIS2_PLACEMENT_3D('',#28938,#22690,#22691);
#20117=AXIS2_PLACEMENT_3D('',#28941,#22692,#22693);
#20118=AXIS2_PLACEMENT_3D('',#28943,#22694,#22695);
#20119=AXIS2_PLACEMENT_3D('',#28945,#22696,#22697);
#20120=AXIS2_PLACEMENT_3D('',#28949,#22699,#22700);
#20121=AXIS2_PLACEMENT_3D('',#28951,#22701,#22702);
#20122=AXIS2_PLACEMENT_3D('',#28953,#22703,#22704);
#20123=AXIS2_PLACEMENT_3D('',#28997,#22708,#22709);
#20124=AXIS2_PLACEMENT_3D('',#29003,#22713,#22714);
#20125=AXIS2_PLACEMENT_3D('',#29006,#22716,#22717);
#20126=AXIS2_PLACEMENT_3D('',#29007,#22718,#22719);
#20127=AXIS2_PLACEMENT_3D('',#29010,#22721,#22722);
#20128=AXIS2_PLACEMENT_3D('',#29011,#22723,#22724);
#20129=AXIS2_PLACEMENT_3D('',#29013,#22725,#22726);
#20130=AXIS2_PLACEMENT_3D('',#29015,#22728,#22729);
#20131=AXIS2_PLACEMENT_3D('',#29019,#22732,#22733);
#20132=AXIS2_PLACEMENT_3D('',#29022,#22735,#22736);
#20133=AXIS2_PLACEMENT_3D('',#29023,#22737,#22738);
#20134=AXIS2_PLACEMENT_3D('',#29025,#22739,#22740);
#20135=AXIS2_PLACEMENT_3D('',#29026,#22741,#22742);
#20136=AXIS2_PLACEMENT_3D('',#29027,#22743,#22744);
#20137=AXIS2_PLACEMENT_3D('',#29029,#22746,#22747);
#20138=AXIS2_PLACEMENT_3D('',#29030,#22748,#22749);
#20139=AXIS2_PLACEMENT_3D('',#29036,#22753,#22754);
#20140=AXIS2_PLACEMENT_3D('',#29039,#22756,#22757);
#20141=AXIS2_PLACEMENT_3D('',#29040,#22758,#22759);
#20142=AXIS2_PLACEMENT_3D('',#29042,#22760,#22761);
#20143=AXIS2_PLACEMENT_3D('',#29044,#22763,#22764);
#20144=AXIS2_PLACEMENT_3D('',#29046,#22766,#22767);
#20145=AXIS2_PLACEMENT_3D('',#29049,#22768,#22769);
#20146=AXIS2_PLACEMENT_3D('',#29051,#22770,#22771);
#20147=AXIS2_PLACEMENT_3D('',#29053,#22772,#22773);
#20148=AXIS2_PLACEMENT_3D('',#29057,#22775,#22776);
#20149=AXIS2_PLACEMENT_3D('',#29059,#22777,#22778);
#20150=AXIS2_PLACEMENT_3D('',#29061,#22779,#22780);
#20151=AXIS2_PLACEMENT_3D('',#29105,#22784,#22785);
#20152=AXIS2_PLACEMENT_3D('',#29111,#22789,#22790);
#20153=AXIS2_PLACEMENT_3D('',#29114,#22792,#22793);
#20154=AXIS2_PLACEMENT_3D('',#29115,#22794,#22795);
#20155=AXIS2_PLACEMENT_3D('',#29118,#22797,#22798);
#20156=AXIS2_PLACEMENT_3D('',#29119,#22799,#22800);
#20157=AXIS2_PLACEMENT_3D('',#29121,#22801,#22802);
#20158=AXIS2_PLACEMENT_3D('',#29123,#22804,#22805);
#20159=AXIS2_PLACEMENT_3D('',#29127,#22808,#22809);
#20160=AXIS2_PLACEMENT_3D('',#29130,#22811,#22812);
#20161=AXIS2_PLACEMENT_3D('',#29131,#22813,#22814);
#20162=AXIS2_PLACEMENT_3D('',#29133,#22815,#22816);
#20163=AXIS2_PLACEMENT_3D('',#29134,#22817,#22818);
#20164=AXIS2_PLACEMENT_3D('',#29135,#22819,#22820);
#20165=AXIS2_PLACEMENT_3D('',#29137,#22822,#22823);
#20166=AXIS2_PLACEMENT_3D('',#29138,#22824,#22825);
#20167=AXIS2_PLACEMENT_3D('',#29144,#22829,#22830);
#20168=AXIS2_PLACEMENT_3D('',#29147,#22832,#22833);
#20169=AXIS2_PLACEMENT_3D('',#29148,#22834,#22835);
#20170=AXIS2_PLACEMENT_3D('',#29150,#22836,#22837);
#20171=AXIS2_PLACEMENT_3D('',#29152,#22839,#22840);
#20172=AXIS2_PLACEMENT_3D('',#29154,#22842,#22843);
#20173=AXIS2_PLACEMENT_3D('',#29157,#22844,#22845);
#20174=AXIS2_PLACEMENT_3D('',#29159,#22846,#22847);
#20175=AXIS2_PLACEMENT_3D('',#29161,#22848,#22849);
#20176=AXIS2_PLACEMENT_3D('',#29165,#22851,#22852);
#20177=AXIS2_PLACEMENT_3D('',#29167,#22853,#22854);
#20178=AXIS2_PLACEMENT_3D('',#29169,#22855,#22856);
#20179=AXIS2_PLACEMENT_3D('',#29213,#22860,#22861);
#20180=AXIS2_PLACEMENT_3D('',#29219,#22865,#22866);
#20181=AXIS2_PLACEMENT_3D('',#29222,#22868,#22869);
#20182=AXIS2_PLACEMENT_3D('',#29223,#22870,#22871);
#20183=AXIS2_PLACEMENT_3D('',#29226,#22873,#22874);
#20184=AXIS2_PLACEMENT_3D('',#29227,#22875,#22876);
#20185=AXIS2_PLACEMENT_3D('',#29229,#22877,#22878);
#20186=AXIS2_PLACEMENT_3D('',#29231,#22880,#22881);
#20187=AXIS2_PLACEMENT_3D('',#29235,#22884,#22885);
#20188=AXIS2_PLACEMENT_3D('',#29238,#22887,#22888);
#20189=AXIS2_PLACEMENT_3D('',#29239,#22889,#22890);
#20190=AXIS2_PLACEMENT_3D('',#29241,#22891,#22892);
#20191=AXIS2_PLACEMENT_3D('',#29242,#22893,#22894);
#20192=AXIS2_PLACEMENT_3D('',#29243,#22895,#22896);
#20193=AXIS2_PLACEMENT_3D('',#29245,#22898,#22899);
#20194=AXIS2_PLACEMENT_3D('',#29246,#22900,#22901);
#20195=AXIS2_PLACEMENT_3D('',#29252,#22905,#22906);
#20196=AXIS2_PLACEMENT_3D('',#29255,#22908,#22909);
#20197=AXIS2_PLACEMENT_3D('',#29256,#22910,#22911);
#20198=AXIS2_PLACEMENT_3D('',#29258,#22912,#22913);
#20199=AXIS2_PLACEMENT_3D('',#29260,#22915,#22916);
#20200=AXIS2_PLACEMENT_3D('',#29262,#22918,#22919);
#20201=AXIS2_PLACEMENT_3D('',#29265,#22920,#22921);
#20202=AXIS2_PLACEMENT_3D('',#29267,#22922,#22923);
#20203=AXIS2_PLACEMENT_3D('',#29269,#22924,#22925);
#20204=AXIS2_PLACEMENT_3D('',#29273,#22927,#22928);
#20205=AXIS2_PLACEMENT_3D('',#29275,#22929,#22930);
#20206=AXIS2_PLACEMENT_3D('',#29277,#22931,#22932);
#20207=AXIS2_PLACEMENT_3D('',#29321,#22936,#22937);
#20208=AXIS2_PLACEMENT_3D('',#29327,#22941,#22942);
#20209=AXIS2_PLACEMENT_3D('',#29330,#22944,#22945);
#20210=AXIS2_PLACEMENT_3D('',#29331,#22946,#22947);
#20211=AXIS2_PLACEMENT_3D('',#29334,#22949,#22950);
#20212=AXIS2_PLACEMENT_3D('',#29335,#22951,#22952);
#20213=AXIS2_PLACEMENT_3D('',#29337,#22953,#22954);
#20214=AXIS2_PLACEMENT_3D('',#29339,#22956,#22957);
#20215=AXIS2_PLACEMENT_3D('',#29343,#22960,#22961);
#20216=AXIS2_PLACEMENT_3D('',#29346,#22963,#22964);
#20217=AXIS2_PLACEMENT_3D('',#29347,#22965,#22966);
#20218=AXIS2_PLACEMENT_3D('',#29349,#22967,#22968);
#20219=AXIS2_PLACEMENT_3D('',#29350,#22969,#22970);
#20220=AXIS2_PLACEMENT_3D('',#29351,#22971,#22972);
#20221=AXIS2_PLACEMENT_3D('',#29353,#22974,#22975);
#20222=AXIS2_PLACEMENT_3D('',#29354,#22976,#22977);
#20223=AXIS2_PLACEMENT_3D('',#29360,#22981,#22982);
#20224=AXIS2_PLACEMENT_3D('',#29363,#22984,#22985);
#20225=AXIS2_PLACEMENT_3D('',#29364,#22986,#22987);
#20226=AXIS2_PLACEMENT_3D('',#29366,#22988,#22989);
#20227=AXIS2_PLACEMENT_3D('',#29368,#22991,#22992);
#20228=AXIS2_PLACEMENT_3D('',#29370,#22994,#22995);
#20229=AXIS2_PLACEMENT_3D('',#29373,#22996,#22997);
#20230=AXIS2_PLACEMENT_3D('',#29375,#22998,#22999);
#20231=AXIS2_PLACEMENT_3D('',#29377,#23000,#23001);
#20232=AXIS2_PLACEMENT_3D('',#29381,#23003,#23004);
#20233=AXIS2_PLACEMENT_3D('',#29383,#23005,#23006);
#20234=AXIS2_PLACEMENT_3D('',#29385,#23007,#23008);
#20235=AXIS2_PLACEMENT_3D('',#29429,#23012,#23013);
#20236=AXIS2_PLACEMENT_3D('',#29435,#23017,#23018);
#20237=AXIS2_PLACEMENT_3D('',#29438,#23020,#23021);
#20238=AXIS2_PLACEMENT_3D('',#29439,#23022,#23023);
#20239=AXIS2_PLACEMENT_3D('',#29442,#23025,#23026);
#20240=AXIS2_PLACEMENT_3D('',#29443,#23027,#23028);
#20241=AXIS2_PLACEMENT_3D('',#29445,#23029,#23030);
#20242=AXIS2_PLACEMENT_3D('',#29447,#23032,#23033);
#20243=AXIS2_PLACEMENT_3D('',#29451,#23036,#23037);
#20244=AXIS2_PLACEMENT_3D('',#29454,#23039,#23040);
#20245=AXIS2_PLACEMENT_3D('',#29455,#23041,#23042);
#20246=AXIS2_PLACEMENT_3D('',#29457,#23043,#23044);
#20247=AXIS2_PLACEMENT_3D('',#29458,#23045,#23046);
#20248=AXIS2_PLACEMENT_3D('',#29459,#23047,#23048);
#20249=AXIS2_PLACEMENT_3D('',#29461,#23050,#23051);
#20250=AXIS2_PLACEMENT_3D('',#29462,#23052,#23053);
#20251=AXIS2_PLACEMENT_3D('',#29468,#23057,#23058);
#20252=AXIS2_PLACEMENT_3D('',#29471,#23060,#23061);
#20253=AXIS2_PLACEMENT_3D('',#29472,#23062,#23063);
#20254=AXIS2_PLACEMENT_3D('',#29474,#23064,#23065);
#20255=AXIS2_PLACEMENT_3D('',#29476,#23067,#23068);
#20256=AXIS2_PLACEMENT_3D('',#29478,#23070,#23071);
#20257=AXIS2_PLACEMENT_3D('',#29481,#23072,#23073);
#20258=AXIS2_PLACEMENT_3D('',#29483,#23074,#23075);
#20259=AXIS2_PLACEMENT_3D('',#29485,#23076,#23077);
#20260=AXIS2_PLACEMENT_3D('',#29489,#23079,#23080);
#20261=AXIS2_PLACEMENT_3D('',#29491,#23081,#23082);
#20262=AXIS2_PLACEMENT_3D('',#29493,#23083,#23084);
#20263=AXIS2_PLACEMENT_3D('',#29537,#23088,#23089);
#20264=AXIS2_PLACEMENT_3D('',#29543,#23093,#23094);
#20265=AXIS2_PLACEMENT_3D('',#29546,#23096,#23097);
#20266=AXIS2_PLACEMENT_3D('',#29547,#23098,#23099);
#20267=AXIS2_PLACEMENT_3D('',#29550,#23101,#23102);
#20268=AXIS2_PLACEMENT_3D('',#29551,#23103,#23104);
#20269=AXIS2_PLACEMENT_3D('',#29553,#23105,#23106);
#20270=AXIS2_PLACEMENT_3D('',#29555,#23108,#23109);
#20271=AXIS2_PLACEMENT_3D('',#29559,#23112,#23113);
#20272=AXIS2_PLACEMENT_3D('',#29562,#23115,#23116);
#20273=AXIS2_PLACEMENT_3D('',#29563,#23117,#23118);
#20274=AXIS2_PLACEMENT_3D('',#29565,#23119,#23120);
#20275=AXIS2_PLACEMENT_3D('',#29566,#23121,#23122);
#20276=AXIS2_PLACEMENT_3D('',#29567,#23123,#23124);
#20277=AXIS2_PLACEMENT_3D('',#29569,#23126,#23127);
#20278=AXIS2_PLACEMENT_3D('',#29570,#23128,#23129);
#20279=AXIS2_PLACEMENT_3D('',#29576,#23133,#23134);
#20280=AXIS2_PLACEMENT_3D('',#29579,#23136,#23137);
#20281=AXIS2_PLACEMENT_3D('',#29580,#23138,#23139);
#20282=AXIS2_PLACEMENT_3D('',#29582,#23140,#23141);
#20283=AXIS2_PLACEMENT_3D('',#29584,#23142,#23143);
#20284=AXIS2_PLACEMENT_3D('',#29586,#23144,#23145);
#20285=AXIS2_PLACEMENT_3D('',#29588,#23147,#23148);
#20286=AXIS2_PLACEMENT_3D('',#29590,#23150,#23151);
#20287=AXIS2_PLACEMENT_3D('',#29623,#23168,#23169);
#20288=AXIS2_PLACEMENT_3D('',#29629,#23173,#23174);
#20289=AXIS2_PLACEMENT_3D('',#29633,#23177,#23178);
#20290=AXIS2_PLACEMENT_3D('',#29639,#23182,#23183);
#20291=AXIS2_PLACEMENT_3D('',#29647,#23188,#23189);
#20292=AXIS2_PLACEMENT_3D('',#29651,#23192,#23193);
#20293=AXIS2_PLACEMENT_3D('',#29655,#23196,#23197);
#20294=AXIS2_PLACEMENT_3D('',#29657,#23199,#23200);
#20295=AXIS2_PLACEMENT_3D('',#29687,#23216,#23217);
#20296=AXIS2_PLACEMENT_3D('',#29690,#23220,#23221);
#20297=AXIS2_PLACEMENT_3D('',#29692,#23223,#23224);
#20298=AXIS2_PLACEMENT_3D('',#29694,#23226,#23227);
#20299=AXIS2_PLACEMENT_3D('',#29696,#23229,#23230);
#20300=AXIS2_PLACEMENT_3D('',#29698,#23232,#23233);
#20301=AXIS2_PLACEMENT_3D('',#29700,#23235,#23236);
#20302=AXIS2_PLACEMENT_3D('',#29702,#23238,#23239);
#20303=AXIS2_PLACEMENT_3D('',#29713,#23246,#23247);
#20304=AXIS2_PLACEMENT_3D('',#29722,#23253,#23254);
#20305=AXIS2_PLACEMENT_3D('',#29731,#23260,#23261);
#20306=AXIS2_PLACEMENT_3D('',#29732,#23262,#23263);
#20307=AXIS2_PLACEMENT_3D('',#29740,#23269,#23270);
#20308=AXIS2_PLACEMENT_3D('',#29743,#23273,#23274);
#20309=AXIS2_PLACEMENT_3D('',#29746,#23277,#23278);
#20310=AXIS2_PLACEMENT_3D('',#29747,#23279,#23280);
#20311=AXIS2_PLACEMENT_3D('',#29748,#23281,#23282);
#20312=AXIS2_PLACEMENT_3D('',#29749,#23283,#23284);
#20313=AXIS2_PLACEMENT_3D('',#29750,#23285,#23286);
#20314=AXIS2_PLACEMENT_3D('',#29752,#23288,#23289);
#20315=AXIS2_PLACEMENT_3D('',#29753,#23290,#23291);
#20316=AXIS2_PLACEMENT_3D('',#29754,#23292,#23293);
#20317=AXIS2_PLACEMENT_3D('',#29759,#23295,#23296);
#20318=AXIS2_PLACEMENT_3D('',#29762,#23298,#23299);
#20319=AXIS2_PLACEMENT_3D('',#29763,#23300,#23301);
#20320=AXIS2_PLACEMENT_3D('',#29768,#23303,#23304);
#20321=AXIS2_PLACEMENT_3D('',#29771,#23306,#23307);
#20322=AXIS2_PLACEMENT_3D('',#29772,#23308,#23309);
#20323=AXIS2_PLACEMENT_3D('',#29777,#23311,#23312);
#20324=AXIS2_PLACEMENT_3D('',#29780,#23314,#23315);
#20325=AXIS2_PLACEMENT_3D('',#29781,#23316,#23317);
#20326=AXIS2_PLACEMENT_3D('',#29786,#23319,#23320);
#20327=AXIS2_PLACEMENT_3D('',#29789,#23322,#23323);
#20328=AXIS2_PLACEMENT_3D('',#29790,#23324,#23325);
#20329=AXIS2_PLACEMENT_3D('',#29795,#23327,#23328);
#20330=AXIS2_PLACEMENT_3D('',#29798,#23330,#23331);
#20331=AXIS2_PLACEMENT_3D('',#29799,#23332,#23333);
#20332=AXIS2_PLACEMENT_3D('',#29804,#23335,#23336);
#20333=AXIS2_PLACEMENT_3D('',#29807,#23338,#23339);
#20334=AXIS2_PLACEMENT_3D('',#29808,#23340,#23341);
#20335=AXIS2_PLACEMENT_3D('',#29813,#23343,#23344);
#20336=AXIS2_PLACEMENT_3D('',#29816,#23346,#23347);
#20337=AXIS2_PLACEMENT_3D('',#29817,#23348,#23349);
#20338=AXIS2_PLACEMENT_3D('',#29822,#23351,#23352);
#20339=AXIS2_PLACEMENT_3D('',#29825,#23354,#23355);
#20340=AXIS2_PLACEMENT_3D('',#29826,#23356,#23357);
#20341=AXIS2_PLACEMENT_3D('',#29831,#23359,#23360);
#20342=AXIS2_PLACEMENT_3D('',#29834,#23362,#23363);
#20343=AXIS2_PLACEMENT_3D('',#29835,#23364,#23365);
#20344=AXIS2_PLACEMENT_3D('',#29840,#23367,#23368);
#20345=AXIS2_PLACEMENT_3D('',#29843,#23370,#23371);
#20346=AXIS2_PLACEMENT_3D('',#29844,#23372,#23373);
#20347=AXIS2_PLACEMENT_3D('',#29849,#23375,#23376);
#20348=AXIS2_PLACEMENT_3D('',#29852,#23378,#23379);
#20349=AXIS2_PLACEMENT_3D('',#29853,#23380,#23381);
#20350=AXIS2_PLACEMENT_3D('',#29858,#23383,#23384);
#20351=AXIS2_PLACEMENT_3D('',#29861,#23386,#23387);
#20352=AXIS2_PLACEMENT_3D('',#29862,#23388,#23389);
#20353=AXIS2_PLACEMENT_3D('',#29867,#23391,#23392);
#20354=AXIS2_PLACEMENT_3D('',#29870,#23394,#23395);
#20355=AXIS2_PLACEMENT_3D('',#29871,#23396,#23397);
#20356=AXIS2_PLACEMENT_3D('',#29876,#23399,#23400);
#20357=AXIS2_PLACEMENT_3D('',#29879,#23402,#23403);
#20358=AXIS2_PLACEMENT_3D('',#29880,#23404,#23405);
#20359=AXIS2_PLACEMENT_3D('',#29885,#23407,#23408);
#20360=AXIS2_PLACEMENT_3D('',#29888,#23410,#23411);
#20361=AXIS2_PLACEMENT_3D('',#29889,#23412,#23413);
#20362=AXIS2_PLACEMENT_3D('',#29894,#23415,#23416);
#20363=AXIS2_PLACEMENT_3D('',#29897,#23418,#23419);
#20364=AXIS2_PLACEMENT_3D('',#29898,#23420,#23421);
#20365=AXIS2_PLACEMENT_3D('',#29903,#23423,#23424);
#20366=AXIS2_PLACEMENT_3D('',#29906,#23426,#23427);
#20367=AXIS2_PLACEMENT_3D('',#29907,#23428,#23429);
#20368=AXIS2_PLACEMENT_3D('',#29912,#23431,#23432);
#20369=AXIS2_PLACEMENT_3D('',#29915,#23434,#23435);
#20370=AXIS2_PLACEMENT_3D('',#29916,#23436,#23437);
#20371=AXIS2_PLACEMENT_3D('',#29921,#23439,#23440);
#20372=AXIS2_PLACEMENT_3D('',#29924,#23442,#23443);
#20373=AXIS2_PLACEMENT_3D('',#29925,#23444,#23445);
#20374=AXIS2_PLACEMENT_3D('',#29930,#23447,#23448);
#20375=AXIS2_PLACEMENT_3D('',#29933,#23450,#23451);
#20376=AXIS2_PLACEMENT_3D('',#29934,#23452,#23453);
#20377=AXIS2_PLACEMENT_3D('',#29939,#23455,#23456);
#20378=AXIS2_PLACEMENT_3D('',#29942,#23458,#23459);
#20379=AXIS2_PLACEMENT_3D('',#29943,#23460,#23461);
#20380=AXIS2_PLACEMENT_3D('',#29948,#23463,#23464);
#20381=AXIS2_PLACEMENT_3D('',#29951,#23466,#23467);
#20382=AXIS2_PLACEMENT_3D('',#29952,#23468,#23469);
#20383=AXIS2_PLACEMENT_3D('',#29957,#23471,#23472);
#20384=AXIS2_PLACEMENT_3D('',#29960,#23474,#23475);
#20385=AXIS2_PLACEMENT_3D('',#29961,#23476,#23477);
#20386=AXIS2_PLACEMENT_3D('',#29966,#23479,#23480);
#20387=AXIS2_PLACEMENT_3D('',#29969,#23482,#23483);
#20388=AXIS2_PLACEMENT_3D('',#29970,#23484,#23485);
#20389=AXIS2_PLACEMENT_3D('',#29975,#23487,#23488);
#20390=AXIS2_PLACEMENT_3D('',#29978,#23490,#23491);
#20391=AXIS2_PLACEMENT_3D('',#29979,#23492,#23493);
#20392=AXIS2_PLACEMENT_3D('',#29984,#23495,#23496);
#20393=AXIS2_PLACEMENT_3D('',#29987,#23498,#23499);
#20394=AXIS2_PLACEMENT_3D('',#29988,#23500,#23501);
#20395=AXIS2_PLACEMENT_3D('',#29993,#23503,#23504);
#20396=AXIS2_PLACEMENT_3D('',#29996,#23506,#23507);
#20397=AXIS2_PLACEMENT_3D('',#29997,#23508,#23509);
#20398=AXIS2_PLACEMENT_3D('',#30002,#23511,#23512);
#20399=AXIS2_PLACEMENT_3D('',#30005,#23514,#23515);
#20400=AXIS2_PLACEMENT_3D('',#30006,#23516,#23517);
#20401=AXIS2_PLACEMENT_3D('',#30011,#23519,#23520);
#20402=AXIS2_PLACEMENT_3D('',#30014,#23522,#23523);
#20403=AXIS2_PLACEMENT_3D('',#30015,#23524,#23525);
#20404=AXIS2_PLACEMENT_3D('',#30020,#23527,#23528);
#20405=AXIS2_PLACEMENT_3D('',#30023,#23530,#23531);
#20406=AXIS2_PLACEMENT_3D('',#30024,#23532,#23533);
#20407=AXIS2_PLACEMENT_3D('',#30029,#23535,#23536);
#20408=AXIS2_PLACEMENT_3D('',#30032,#23538,#23539);
#20409=AXIS2_PLACEMENT_3D('',#30033,#23540,#23541);
#20410=AXIS2_PLACEMENT_3D('',#30038,#23543,#23544);
#20411=AXIS2_PLACEMENT_3D('',#30041,#23546,#23547);
#20412=AXIS2_PLACEMENT_3D('',#30042,#23548,#23549);
#20413=AXIS2_PLACEMENT_3D('',#30047,#23551,#23552);
#20414=AXIS2_PLACEMENT_3D('',#30050,#23554,#23555);
#20415=AXIS2_PLACEMENT_3D('',#30051,#23556,#23557);
#20416=AXIS2_PLACEMENT_3D('',#30056,#23559,#23560);
#20417=AXIS2_PLACEMENT_3D('',#30059,#23562,#23563);
#20418=AXIS2_PLACEMENT_3D('',#30060,#23564,#23565);
#20419=AXIS2_PLACEMENT_3D('',#30065,#23567,#23568);
#20420=AXIS2_PLACEMENT_3D('',#30068,#23570,#23571);
#20421=AXIS2_PLACEMENT_3D('',#30069,#23572,#23573);
#20422=AXIS2_PLACEMENT_3D('',#30074,#23575,#23576);
#20423=AXIS2_PLACEMENT_3D('',#30077,#23578,#23579);
#20424=AXIS2_PLACEMENT_3D('',#30078,#23580,#23581);
#20425=AXIS2_PLACEMENT_3D('',#30083,#23583,#23584);
#20426=AXIS2_PLACEMENT_3D('',#30086,#23586,#23587);
#20427=AXIS2_PLACEMENT_3D('',#30087,#23588,#23589);
#20428=AXIS2_PLACEMENT_3D('',#30092,#23591,#23592);
#20429=AXIS2_PLACEMENT_3D('',#30095,#23594,#23595);
#20430=AXIS2_PLACEMENT_3D('',#30096,#23596,#23597);
#20431=AXIS2_PLACEMENT_3D('',#30101,#23599,#23600);
#20432=AXIS2_PLACEMENT_3D('',#30104,#23602,#23603);
#20433=AXIS2_PLACEMENT_3D('',#30105,#23604,#23605);
#20434=AXIS2_PLACEMENT_3D('',#30110,#23607,#23608);
#20435=AXIS2_PLACEMENT_3D('',#30113,#23610,#23611);
#20436=AXIS2_PLACEMENT_3D('',#30114,#23612,#23613);
#20437=AXIS2_PLACEMENT_3D('',#30119,#23615,#23616);
#20438=AXIS2_PLACEMENT_3D('',#30122,#23618,#23619);
#20439=AXIS2_PLACEMENT_3D('',#30123,#23620,#23621);
#20440=AXIS2_PLACEMENT_3D('',#30128,#23623,#23624);
#20441=AXIS2_PLACEMENT_3D('',#30131,#23626,#23627);
#20442=AXIS2_PLACEMENT_3D('',#30132,#23628,#23629);
#20443=AXIS2_PLACEMENT_3D('',#30137,#23631,#23632);
#20444=AXIS2_PLACEMENT_3D('',#30140,#23634,#23635);
#20445=AXIS2_PLACEMENT_3D('',#30141,#23636,#23637);
#20446=AXIS2_PLACEMENT_3D('',#30146,#23639,#23640);
#20447=AXIS2_PLACEMENT_3D('',#30149,#23642,#23643);
#20448=AXIS2_PLACEMENT_3D('',#30150,#23644,#23645);
#20449=AXIS2_PLACEMENT_3D('',#30152,#23646,#23647);
#20450=AXIS2_PLACEMENT_3D('',#30154,#23648,#23649);
#20451=AXIS2_PLACEMENT_3D('',#30155,#23650,#23651);
#20452=AXIS2_PLACEMENT_3D('',#30156,#23652,#23653);
#20453=AXIS2_PLACEMENT_3D('',#30157,#23654,#23655);
#20454=AXIS2_PLACEMENT_3D('',#30158,#23656,#23657);
#20455=AXIS2_PLACEMENT_3D('',#30159,#23658,#23659);
#20456=AXIS2_PLACEMENT_3D('',#30160,#23660,#23661);
#20457=AXIS2_PLACEMENT_3D('',#30161,#23662,#23663);
#20458=AXIS2_PLACEMENT_3D('',#30162,#23664,#23665);
#20459=AXIS2_PLACEMENT_3D('',#30163,#23666,#23667);
#20460=AXIS2_PLACEMENT_3D('',#30164,#23668,#23669);
#20461=AXIS2_PLACEMENT_3D('',#30165,#23670,#23671);
#20462=AXIS2_PLACEMENT_3D('',#30166,#23672,#23673);
#20463=AXIS2_PLACEMENT_3D('',#30167,#23674,#23675);
#20464=AXIS2_PLACEMENT_3D('',#30168,#23676,#23677);
#20465=AXIS2_PLACEMENT_3D('',#30169,#23678,#23679);
#20466=AXIS2_PLACEMENT_3D('',#30170,#23680,#23681);
#20467=AXIS2_PLACEMENT_3D('',#30171,#23682,#23683);
#20468=AXIS2_PLACEMENT_3D('',#30172,#23684,#23685);
#20469=AXIS2_PLACEMENT_3D('',#30173,#23686,#23687);
#20470=AXIS2_PLACEMENT_3D('',#30174,#23688,#23689);
#20471=AXIS2_PLACEMENT_3D('',#30175,#23690,#23691);
#20472=AXIS2_PLACEMENT_3D('',#30176,#23692,#23693);
#20473=AXIS2_PLACEMENT_3D('',#30177,#23694,#23695);
#20474=AXIS2_PLACEMENT_3D('',#30178,#23696,#23697);
#20475=AXIS2_PLACEMENT_3D('',#30179,#23698,#23699);
#20476=AXIS2_PLACEMENT_3D('',#30180,#23700,#23701);
#20477=AXIS2_PLACEMENT_3D('',#30181,#23702,#23703);
#20478=AXIS2_PLACEMENT_3D('',#30182,#23704,#23705);
#20479=AXIS2_PLACEMENT_3D('',#30183,#23706,#23707);
#20480=AXIS2_PLACEMENT_3D('',#30184,#23708,#23709);
#20481=AXIS2_PLACEMENT_3D('',#30185,#23710,#23711);
#20482=AXIS2_PLACEMENT_3D('',#30186,#23712,#23713);
#20483=AXIS2_PLACEMENT_3D('',#30187,#23714,#23715);
#20484=AXIS2_PLACEMENT_3D('',#30188,#23716,#23717);
#20485=AXIS2_PLACEMENT_3D('',#30189,#23718,#23719);
#20486=AXIS2_PLACEMENT_3D('',#30190,#23720,#23721);
#20487=AXIS2_PLACEMENT_3D('',#30191,#23722,#23723);
#20488=AXIS2_PLACEMENT_3D('',#30192,#23724,#23725);
#20489=AXIS2_PLACEMENT_3D('',#30193,#23726,#23727);
#20490=AXIS2_PLACEMENT_3D('',#30194,#23728,#23729);
#20491=AXIS2_PLACEMENT_3D('',#30195,#23730,#23731);
#20492=AXIS2_PLACEMENT_3D('',#30196,#23732,#23733);
#20493=AXIS2_PLACEMENT_3D('',#30197,#23734,#23735);
#20494=AXIS2_PLACEMENT_3D('',#30198,#23736,#23737);
#20495=AXIS2_PLACEMENT_3D('',#30200,#23738,#23739);
#20496=AXIS2_PLACEMENT_3D('',#30201,#23740,#23741);
#20497=AXIS2_PLACEMENT_3D('',#30203,#23742,#23743);
#20498=AXIS2_PLACEMENT_3D('',#30205,#23745,#23746);
#20499=AXIS2_PLACEMENT_3D('',#30208,#23748,#23749);
#20500=AXIS2_PLACEMENT_3D('',#30209,#23750,#23751);
#20501=AXIS2_PLACEMENT_3D('',#30210,#23752,#23753);
#20502=AXIS2_PLACEMENT_3D('',#30211,#23754,#23755);
#20503=AXIS2_PLACEMENT_3D('',#30212,#23756,#23757);
#20504=AXIS2_PLACEMENT_3D('',#30213,#23758,#23759);
#20505=AXIS2_PLACEMENT_3D('',#30214,#23760,#23761);
#20506=AXIS2_PLACEMENT_3D('',#30215,#23762,#23763);
#20507=AXIS2_PLACEMENT_3D('',#30216,#23764,#23765);
#20508=AXIS2_PLACEMENT_3D('',#30217,#23766,#23767);
#20509=AXIS2_PLACEMENT_3D('',#30218,#23768,#23769);
#20510=AXIS2_PLACEMENT_3D('',#30219,#23770,#23771);
#20511=AXIS2_PLACEMENT_3D('',#30220,#23772,#23773);
#20512=AXIS2_PLACEMENT_3D('',#30221,#23774,#23775);
#20513=AXIS2_PLACEMENT_3D('',#30222,#23776,#23777);
#20514=AXIS2_PLACEMENT_3D('',#30223,#23778,#23779);
#20515=AXIS2_PLACEMENT_3D('',#30224,#23780,#23781);
#20516=AXIS2_PLACEMENT_3D('',#30225,#23782,#23783);
#20517=AXIS2_PLACEMENT_3D('',#30226,#23784,#23785);
#20518=AXIS2_PLACEMENT_3D('',#30227,#23786,#23787);
#20519=AXIS2_PLACEMENT_3D('',#30228,#23788,#23789);
#20520=AXIS2_PLACEMENT_3D('',#30229,#23790,#23791);
#20521=AXIS2_PLACEMENT_3D('',#30230,#23792,#23793);
#20522=AXIS2_PLACEMENT_3D('',#30231,#23794,#23795);
#20523=AXIS2_PLACEMENT_3D('',#30232,#23796,#23797);
#20524=AXIS2_PLACEMENT_3D('',#30233,#23798,#23799);
#20525=AXIS2_PLACEMENT_3D('',#30234,#23800,#23801);
#20526=AXIS2_PLACEMENT_3D('',#30235,#23802,#23803);
#20527=AXIS2_PLACEMENT_3D('',#30236,#23804,#23805);
#20528=AXIS2_PLACEMENT_3D('',#30237,#23806,#23807);
#20529=AXIS2_PLACEMENT_3D('',#30238,#23808,#23809);
#20530=AXIS2_PLACEMENT_3D('',#30239,#23810,#23811);
#20531=AXIS2_PLACEMENT_3D('',#30240,#23812,#23813);
#20532=AXIS2_PLACEMENT_3D('',#30241,#23814,#23815);
#20533=AXIS2_PLACEMENT_3D('',#30242,#23816,#23817);
#20534=AXIS2_PLACEMENT_3D('',#30243,#23818,#23819);
#20535=AXIS2_PLACEMENT_3D('',#30244,#23820,#23821);
#20536=AXIS2_PLACEMENT_3D('',#30245,#23822,#23823);
#20537=AXIS2_PLACEMENT_3D('',#30246,#23824,#23825);
#20538=AXIS2_PLACEMENT_3D('',#30247,#23826,#23827);
#20539=AXIS2_PLACEMENT_3D('',#30248,#23828,#23829);
#20540=AXIS2_PLACEMENT_3D('',#30249,#23830,#23831);
#20541=AXIS2_PLACEMENT_3D('',#30250,#23832,#23833);
#20542=AXIS2_PLACEMENT_3D('',#30251,#23834,#23835);
#20543=AXIS2_PLACEMENT_3D('',#30252,#23836,#23837);
#20544=AXIS2_PLACEMENT_3D('',#30253,#23838,#23839);
#20545=AXIS2_PLACEMENT_3D('',#30254,#23840,#23841);
#20546=AXIS2_PLACEMENT_3D('',#30255,#23842,#23843);
#20547=AXIS2_PLACEMENT_3D('',#30256,#23844,#23845);
#20548=AXIS2_PLACEMENT_3D('',#30257,#23846,#23847);
#20549=AXIS2_PLACEMENT_3D('',#30258,#23848,#23849);
#20550=AXIS2_PLACEMENT_3D('',#30259,#23850,#23851);
#20551=AXIS2_PLACEMENT_3D('',#30260,#23852,#23853);
#20552=AXIS2_PLACEMENT_3D('',#30261,#23854,#23855);
#20553=AXIS2_PLACEMENT_3D('',#30262,#23856,#23857);
#20554=AXIS2_PLACEMENT_3D('',#30263,#23858,#23859);
#20555=AXIS2_PLACEMENT_3D('',#30264,#23860,#23861);
#20556=AXIS2_PLACEMENT_3D('',#30265,#23862,#23863);
#20557=AXIS2_PLACEMENT_3D('',#30266,#23864,#23865);
#20558=AXIS2_PLACEMENT_3D('',#30267,#23866,#23867);
#20559=AXIS2_PLACEMENT_3D('',#30268,#23868,#23869);
#20560=AXIS2_PLACEMENT_3D('',#30269,#23870,#23871);
#20561=AXIS2_PLACEMENT_3D('',#30270,#23872,#23873);
#20562=AXIS2_PLACEMENT_3D('',#30271,#23874,#23875);
#20563=AXIS2_PLACEMENT_3D('',#30272,#23876,#23877);
#20564=AXIS2_PLACEMENT_3D('',#30273,#23878,#23879);
#20565=AXIS2_PLACEMENT_3D('',#30274,#23880,#23881);
#20566=AXIS2_PLACEMENT_3D('',#30275,#23882,#23883);
#20567=AXIS2_PLACEMENT_3D('',#30276,#23884,#23885);
#20568=AXIS2_PLACEMENT_3D('',#30277,#23886,#23887);
#20569=AXIS2_PLACEMENT_3D('',#30278,#23888,#23889);
#20570=AXIS2_PLACEMENT_3D('',#30279,#23890,#23891);
#20571=AXIS2_PLACEMENT_3D('',#30280,#23892,#23893);
#20572=AXIS2_PLACEMENT_3D('',#30281,#23894,#23895);
#20573=AXIS2_PLACEMENT_3D('',#30282,#23896,#23897);
#20574=AXIS2_PLACEMENT_3D('',#30283,#23898,#23899);
#20575=AXIS2_PLACEMENT_3D('',#30284,#23900,#23901);
#20576=AXIS2_PLACEMENT_3D('',#30285,#23902,#23903);
#20577=AXIS2_PLACEMENT_3D('',#30286,#23904,#23905);
#20578=AXIS2_PLACEMENT_3D('',#30287,#23906,#23907);
#20579=AXIS2_PLACEMENT_3D('',#30288,#23908,#23909);
#20580=AXIS2_PLACEMENT_3D('',#30289,#23910,#23911);
#20581=AXIS2_PLACEMENT_3D('',#30290,#23912,#23913);
#20582=AXIS2_PLACEMENT_3D('',#30291,#23914,#23915);
#20583=AXIS2_PLACEMENT_3D('',#30292,#23916,#23917);
#20584=AXIS2_PLACEMENT_3D('',#30293,#23918,#23919);
#20585=AXIS2_PLACEMENT_3D('',#30294,#23920,#23921);
#20586=AXIS2_PLACEMENT_3D('',#30295,#23922,#23923);
#20587=AXIS2_PLACEMENT_3D('',#30296,#23924,#23925);
#20588=AXIS2_PLACEMENT_3D('',#30298,#23926,#23927);
#20589=AXIS2_PLACEMENT_3D('',#30299,#23928,#23929);
#20590=AXIS2_PLACEMENT_3D('',#30300,#23930,#23931);
#20591=AXIS2_PLACEMENT_3D('',#30302,#23933,#23934);
#20592=AXIS2_PLACEMENT_3D('',#30303,#23935,#23936);
#20593=AXIS2_PLACEMENT_3D('',#30312,#23941,#23942);
#20594=AXIS2_PLACEMENT_3D('',#30314,#23943,#23944);
#20595=AXIS2_PLACEMENT_3D('',#30316,#23945,#23946);
#20596=AXIS2_PLACEMENT_3D('',#30319,#23948,#23949);
#20597=AXIS2_PLACEMENT_3D('',#30320,#23950,#23951);
#20598=AXIS2_PLACEMENT_3D('',#30322,#23952,#23953);
#20599=AXIS2_PLACEMENT_3D('',#30324,#23954,#23955);
#20600=AXIS2_PLACEMENT_3D('',#30328,#23957,#23958);
#20601=AXIS2_PLACEMENT_3D('',#30330,#23959,#23960);
#20602=AXIS2_PLACEMENT_3D('',#30338,#23961,#23962);
#20603=AXIS2_PLACEMENT_3D('',#30339,#23963,#23964);
#20604=AXIS2_PLACEMENT_3D('',#30341,#23965,#23966);
#20605=AXIS2_PLACEMENT_3D('',#30343,#23967,#23968);
#20606=AXIS2_PLACEMENT_3D('',#30346,#23970,#23971);
#20607=AXIS2_PLACEMENT_3D('',#30347,#23972,#23973);
#20608=AXIS2_PLACEMENT_3D('',#30353,#23977,#23978);
#20609=AXIS2_PLACEMENT_3D('',#30355,#23979,#23980);
#20610=AXIS2_PLACEMENT_3D('',#30357,#23981,#23982);
#20611=AXIS2_PLACEMENT_3D('',#30360,#23984,#23985);
#20612=AXIS2_PLACEMENT_3D('',#30361,#23986,#23987);
#20613=AXIS2_PLACEMENT_3D('',#30363,#23988,#23989);
#20614=AXIS2_PLACEMENT_3D('',#30365,#23990,#23991);
#20615=AXIS2_PLACEMENT_3D('',#30369,#23993,#23994);
#20616=AXIS2_PLACEMENT_3D('',#30371,#23995,#23996);
#20617=AXIS2_PLACEMENT_3D('',#30379,#23997,#23998);
#20618=AXIS2_PLACEMENT_3D('',#30380,#23999,#24000);
#20619=AXIS2_PLACEMENT_3D('',#30382,#24001,#24002);
#20620=AXIS2_PLACEMENT_3D('',#30384,#24003,#24004);
#20621=AXIS2_PLACEMENT_3D('',#30387,#24006,#24007);
#20622=AXIS2_PLACEMENT_3D('',#30388,#24008,#24009);
#20623=AXIS2_PLACEMENT_3D('',#30394,#24013,#24014);
#20624=AXIS2_PLACEMENT_3D('',#30396,#24015,#24016);
#20625=AXIS2_PLACEMENT_3D('',#30398,#24017,#24018);
#20626=AXIS2_PLACEMENT_3D('',#30401,#24020,#24021);
#20627=AXIS2_PLACEMENT_3D('',#30402,#24022,#24023);
#20628=AXIS2_PLACEMENT_3D('',#30404,#24024,#24025);
#20629=AXIS2_PLACEMENT_3D('',#30406,#24026,#24027);
#20630=AXIS2_PLACEMENT_3D('',#30410,#24029,#24030);
#20631=AXIS2_PLACEMENT_3D('',#30412,#24031,#24032);
#20632=AXIS2_PLACEMENT_3D('',#30420,#24033,#24034);
#20633=AXIS2_PLACEMENT_3D('',#30421,#24035,#24036);
#20634=AXIS2_PLACEMENT_3D('',#30430,#24041,#24042);
#20635=AXIS2_PLACEMENT_3D('',#30439,#24047,#24048);
#20636=AXIS2_PLACEMENT_3D('',#30447,#24053,#24054);
#20637=AXIS2_PLACEMENT_3D('',#30456,#24059,#24060);
#20638=AXIS2_PLACEMENT_3D('',#30459,#24061,#24062);
#20639=AXIS2_PLACEMENT_3D('',#30460,#24063,#24064);
#20640=AXIS2_PLACEMENT_3D('',#30462,#24065,#24066);
#20641=AXIS2_PLACEMENT_3D('',#30464,#24068,#24069);
#20642=AXIS2_PLACEMENT_3D('',#30467,#24070,#24071);
#20643=AXIS2_PLACEMENT_3D('',#30469,#24072,#24073);
#20644=AXIS2_PLACEMENT_3D('',#30478,#24074,#24075);
#20645=AXIS2_PLACEMENT_3D('',#30479,#24076,#24077);
#20646=AXIS2_PLACEMENT_3D('',#30481,#24078,#24079);
#20647=AXIS2_PLACEMENT_3D('',#30483,#24081,#24082);
#20648=AXIS2_PLACEMENT_3D('',#30485,#24083,#24084);
#20649=AXIS2_PLACEMENT_3D('',#30486,#24085,#24086);
#20650=AXIS2_PLACEMENT_3D('',#30487,#24087,#24088);
#20651=AXIS2_PLACEMENT_3D('',#30488,#24089,#24090);
#20652=AXIS2_PLACEMENT_3D('',#30490,#24091,#24092);
#20653=AXIS2_PLACEMENT_3D('',#30494,#24094,#24095);
#20654=AXIS2_PLACEMENT_3D('',#30495,#24096,#24097);
#20655=AXIS2_PLACEMENT_3D('',#30496,#24098,#24099);
#20656=AXIS2_PLACEMENT_3D('',#30502,#24103,#24104);
#20657=AXIS2_PLACEMENT_3D('',#30510,#24109,#24110);
#20658=AXIS2_PLACEMENT_3D('',#30512,#24112,#24113);
#20659=AXIS2_PLACEMENT_3D('',#30515,#24114,#24115);
#20660=AXIS2_PLACEMENT_3D('',#30518,#24117,#24118);
#20661=AXIS2_PLACEMENT_3D('',#30519,#24119,#24120);
#20662=AXIS2_PLACEMENT_3D('',#30520,#24121,#24122);
#20663=AXIS2_PLACEMENT_3D('',#30521,#24123,#24124);
#20664=AXIS2_PLACEMENT_3D('',#30523,#24126,#24127);
#20665=AXIS2_PLACEMENT_3D('',#30525,#24129,#24130);
#20666=AXIS2_PLACEMENT_3D('',#30528,#24131,#24132);
#20667=AXIS2_PLACEMENT_3D('',#30531,#24134,#24135);
#20668=AXIS2_PLACEMENT_3D('',#30532,#24136,#24137);
#20669=AXIS2_PLACEMENT_3D('',#30533,#24138,#24139);
#20670=AXIS2_PLACEMENT_3D('',#30534,#24140,#24141);
#20671=AXIS2_PLACEMENT_3D('',#30536,#24143,#24144);
#20672=AXIS2_PLACEMENT_3D('',#30538,#24146,#24147);
#20673=AXIS2_PLACEMENT_3D('',#30541,#24148,#24149);
#20674=AXIS2_PLACEMENT_3D('',#30544,#24151,#24152);
#20675=AXIS2_PLACEMENT_3D('',#30545,#24153,#24154);
#20676=AXIS2_PLACEMENT_3D('',#30546,#24155,#24156);
#20677=AXIS2_PLACEMENT_3D('',#30547,#24157,#24158);
#20678=AXIS2_PLACEMENT_3D('',#30553,#24162,#24163);
#20679=AXIS2_PLACEMENT_3D('',#30559,#24167,#24168);
#20680=AXIS2_PLACEMENT_3D('',#30564,#24172,#24173);
#20681=AXIS2_PLACEMENT_3D('',#30570,#24177,#24178);
#20682=AXIS2_PLACEMENT_3D('',#30578,#24183,#24184);
#20683=AXIS2_PLACEMENT_3D('',#30579,#24185,#24186);
#20684=AXIS2_PLACEMENT_3D('',#30581,#24187,#24188);
#20685=AXIS2_PLACEMENT_3D('',#30582,#24189,#24190);
#20686=AXIS2_PLACEMENT_3D('',#30584,#24191,#24192);
#20687=AXIS2_PLACEMENT_3D('',#30586,#24194,#24195);
#20688=AXIS2_PLACEMENT_3D('',#30588,#24196,#24197);
#20689=AXIS2_PLACEMENT_3D('',#30590,#24199,#24200);
#20690=AXIS2_PLACEMENT_3D('',#30593,#24201,#24202);
#20691=AXIS2_PLACEMENT_3D('',#30595,#24204,#24205);
#20692=AXIS2_PLACEMENT_3D('',#30596,#24206,#24207);
#20693=AXIS2_PLACEMENT_3D('',#30598,#24208,#24209);
#20694=AXIS2_PLACEMENT_3D('',#30600,#24211,#24212);
#20695=AXIS2_PLACEMENT_3D('',#30602,#24213,#24214);
#20696=AXIS2_PLACEMENT_3D('',#30604,#24216,#24217);
#20697=AXIS2_PLACEMENT_3D('',#30607,#24218,#24219);
#20698=AXIS2_PLACEMENT_3D('',#30611,#24221,#24222);
#20699=AXIS2_PLACEMENT_3D('',#30613,#24224,#24225);
#20700=AXIS2_PLACEMENT_3D('',#30618,#24229,#24230);
#20701=AXIS2_PLACEMENT_3D('',#30634,#24238,#24239);
#20702=AXIS2_PLACEMENT_3D('',#30637,#24241,#24242);
#20703=AXIS2_PLACEMENT_3D('',#30639,#24243,#24244);
#20704=AXIS2_PLACEMENT_3D('',#30641,#24245,#24246);
#20705=AXIS2_PLACEMENT_3D('',#30643,#24247,#24248);
#20706=AXIS2_PLACEMENT_3D('',#30644,#24249,#24250);
#20707=AXIS2_PLACEMENT_3D('',#30648,#24252,#24253);
#20708=AXIS2_PLACEMENT_3D('',#30650,#24255,#24256);
#20709=AXIS2_PLACEMENT_3D('',#30662,#24263,#24264);
#20710=AXIS2_PLACEMENT_3D('',#30665,#24267,#24268);
#20711=AXIS2_PLACEMENT_3D('',#30668,#24271,#24272);
#20712=AXIS2_PLACEMENT_3D('',#30672,#24275,#24276);
#20713=AXIS2_PLACEMENT_3D('',#30676,#24279,#24280);
#20714=AXIS2_PLACEMENT_3D('',#30678,#24282,#24283);
#20715=AXIS2_PLACEMENT_3D('',#30684,#24287,#24288);
#20716=AXIS2_PLACEMENT_3D('',#30687,#24289,#24290);
#20717=AXIS2_PLACEMENT_3D('',#30691,#24292,#24293);
#20718=AXIS2_PLACEMENT_3D('',#30693,#24295,#24296);
#20719=AXIS2_PLACEMENT_3D('',#30699,#24300,#24301);
#20720=AXIS2_PLACEMENT_3D('',#30701,#24302,#24303);
#20721=AXIS2_PLACEMENT_3D('',#30704,#24305,#24306);
#20722=AXIS2_PLACEMENT_3D('',#30705,#24307,#24308);
#20723=AXIS2_PLACEMENT_3D('',#30711,#24312,#24313);
#20724=AXIS2_PLACEMENT_3D('',#30713,#24314,#24315);
#20725=AXIS2_PLACEMENT_3D('',#30716,#24317,#24318);
#20726=AXIS2_PLACEMENT_3D('',#30717,#24319,#24320);
#20727=AXIS2_PLACEMENT_3D('',#30723,#24324,#24325);
#20728=AXIS2_PLACEMENT_3D('',#30725,#24326,#24327);
#20729=AXIS2_PLACEMENT_3D('',#30728,#24329,#24330);
#20730=AXIS2_PLACEMENT_3D('',#30729,#24331,#24332);
#20731=AXIS2_PLACEMENT_3D('',#30731,#24334,#24335);
#20732=AXIS2_PLACEMENT_3D('',#30733,#24337,#24338);
#20733=AXIS2_PLACEMENT_3D('',#30734,#24339,#24340);
#20734=AXIS2_PLACEMENT_3D('',#30736,#24342,#24343);
#20735=AXIS2_PLACEMENT_3D('',#30738,#24344,#24345);
#20736=AXIS2_PLACEMENT_3D('',#30740,#24347,#24348);
#20737=AXIS2_PLACEMENT_3D('',#30743,#24351,#24352);
#20738=AXIS2_PLACEMENT_3D('',#30745,#24354,#24355);
#20739=AXIS2_PLACEMENT_3D('',#30748,#24356,#24357);
#20740=AXIS2_PLACEMENT_3D('',#30752,#24359,#24360);
#20741=AXIS2_PLACEMENT_3D('',#30754,#24362,#24363);
#20742=AXIS2_PLACEMENT_3D('',#30756,#24365,#24366);
#20743=AXIS2_PLACEMENT_3D('',#30757,#24367,#24368);
#20744=AXIS2_PLACEMENT_3D('',#30758,#24369,#24370);
#20745=AXIS2_PLACEMENT_3D('',#30759,#24371,#24372);
#20746=AXIS2_PLACEMENT_3D('',#30760,#24373,#24374);
#20747=AXIS2_PLACEMENT_3D('',#30763,#24375,#24376);
#20748=AXIS2_PLACEMENT_3D('',#30767,#24378,#24379);
#20749=AXIS2_PLACEMENT_3D('',#30769,#24381,#24382);
#20750=AXIS2_PLACEMENT_3D('',#30771,#24384,#24385);
#20751=AXIS2_PLACEMENT_3D('',#30776,#24389,#24390);
#20752=AXIS2_PLACEMENT_3D('',#30783,#24395,#24396);
#20753=AXIS2_PLACEMENT_3D('',#30786,#24397,#24398);
#20754=AXIS2_PLACEMENT_3D('',#30790,#24400,#24401);
#20755=AXIS2_PLACEMENT_3D('',#30792,#24403,#24404);
#20756=AXIS2_PLACEMENT_3D('',#30794,#24406,#24407);
#20757=AXIS2_PLACEMENT_3D('',#30801,#24412,#24413);
#20758=AXIS2_PLACEMENT_3D('',#30802,#24414,#24415);
#20759=AXIS2_PLACEMENT_3D('',#30804,#24416,#24417);
#20760=AXIS2_PLACEMENT_3D('',#30807,#24419,#24420);
#20761=AXIS2_PLACEMENT_3D('',#30808,#24421,#24422);
#20762=AXIS2_PLACEMENT_3D('',#30810,#24423,#24424);
#20763=AXIS2_PLACEMENT_3D('',#30811,#24425,#24426);
#20764=AXIS2_PLACEMENT_3D('',#30813,#24427,#24428);
#20765=AXIS2_PLACEMENT_3D('',#30815,#24430,#24431);
#20766=AXIS2_PLACEMENT_3D('',#30818,#24432,#24433);
#20767=AXIS2_PLACEMENT_3D('',#30820,#24435,#24436);
#20768=AXIS2_PLACEMENT_3D('',#30821,#24437,#24438);
#20769=AXIS2_PLACEMENT_3D('',#30824,#24440,#24441);
#20770=AXIS2_PLACEMENT_3D('',#30825,#24442,#24443);
#20771=AXIS2_PLACEMENT_3D('',#30827,#24444,#24445);
#20772=AXIS2_PLACEMENT_3D('',#30828,#24446,#24447);
#20773=AXIS2_PLACEMENT_3D('',#30830,#24449,#24450);
#20774=AXIS2_PLACEMENT_3D('',#30832,#24451,#24452);
#20775=AXIS2_PLACEMENT_3D('',#30833,#24453,#24454);
#20776=AXIS2_PLACEMENT_3D('',#30835,#24456,#24457);
#20777=AXIS2_PLACEMENT_3D('',#30837,#24458,#24459);
#20778=AXIS2_PLACEMENT_3D('',#30838,#24460,#24461);
#20779=AXIS2_PLACEMENT_3D('',#30840,#24463,#24464);
#20780=AXIS2_PLACEMENT_3D('',#30842,#24465,#24466);
#20781=AXIS2_PLACEMENT_3D('',#30843,#24467,#24468);
#20782=AXIS2_PLACEMENT_3D('',#30845,#24470,#24471);
#20783=AXIS2_PLACEMENT_3D('',#30849,#24475,#24476);
#20784=AXIS2_PLACEMENT_3D('',#30851,#24477,#24478);
#20785=AXIS2_PLACEMENT_3D('',#30854,#24480,#24481);
#20786=AXIS2_PLACEMENT_3D('',#30855,#24482,#24483);
#20787=AXIS2_PLACEMENT_3D('',#30856,#24484,#24485);
#20788=AXIS2_PLACEMENT_3D('',#30857,#24486,#24487);
#20789=AXIS2_PLACEMENT_3D('',#30858,#24488,#24489);
#20790=AXIS2_PLACEMENT_3D('',#30859,#24490,#24491);
#20791=AXIS2_PLACEMENT_3D('',#30860,#24492,#24493);
#20792=AXIS2_PLACEMENT_3D('',#30861,#24494,#24495);
#20793=AXIS2_PLACEMENT_3D('',#30862,#24496,#24497);
#20794=AXIS2_PLACEMENT_3D('',#30864,#24498,#24499);
#20795=AXIS2_PLACEMENT_3D('',#30866,#24500,#24501);
#20796=AXIS2_PLACEMENT_3D('',#30868,#24502,#24503);
#20797=AXIS2_PLACEMENT_3D('',#30869,#24504,#24505);
#20798=AXIS2_PLACEMENT_3D('',#30870,#24506,#24507);
#20799=AXIS2_PLACEMENT_3D('',#30874,#24509,#24510);
#20800=AXIS2_PLACEMENT_3D('',#30875,#24511,#24512);
#20801=AXIS2_PLACEMENT_3D('',#30876,#24513,#24514);
#20802=AXIS2_PLACEMENT_3D('',#30878,#24515,#24516);
#20803=AXIS2_PLACEMENT_3D('',#30879,#24517,#24518);
#20804=AXIS2_PLACEMENT_3D('',#30881,#24519,#24520);
#20805=AXIS2_PLACEMENT_3D('',#30882,#24521,#24522);
#20806=AXIS2_PLACEMENT_3D('',#30883,#24523,#24524);
#20807=AXIS2_PLACEMENT_3D('',#30885,#24525,#24526);
#20808=AXIS2_PLACEMENT_3D('',#30886,#24527,#24528);
#20809=AXIS2_PLACEMENT_3D('',#30888,#24530,#24531);
#20810=AXIS2_PLACEMENT_3D('',#30889,#24532,#24533);
#20811=AXIS2_PLACEMENT_3D('',#30898,#24538,#24539);
#20812=AXIS2_PLACEMENT_3D('',#30904,#24543,#24544);
#20813=AXIS2_PLACEMENT_3D('',#30909,#24546,#24547);
#20814=AXIS2_PLACEMENT_3D('',#30912,#24549,#24550);
#20815=AXIS2_PLACEMENT_3D('',#30913,#24551,#24552);
#20816=AXIS2_PLACEMENT_3D('',#30916,#24555,#24556);
#20817=AXIS2_PLACEMENT_3D('',#30922,#24560,#24561);
#20818=AXIS2_PLACEMENT_3D('',#30926,#24564,#24565);
#20819=AXIS2_PLACEMENT_3D('',#30930,#24568,#24569);
#20820=AXIS2_PLACEMENT_3D('',#30932,#24571,#24572);
#20821=AXIS2_PLACEMENT_3D('',#30933,#24573,#24574);
#20822=AXIS2_PLACEMENT_3D('',#30934,#24575,#24576);
#20823=AXIS2_PLACEMENT_3D('',#30943,#24581,#24582);
#20824=AXIS2_PLACEMENT_3D('',#30945,#24583,#24584);
#20825=AXIS2_PLACEMENT_3D('',#30955,#24590,#24591);
#20826=AXIS2_PLACEMENT_3D('',#30958,#24593,#24594);
#20827=AXIS2_PLACEMENT_3D('',#30959,#24595,#24596);
#20828=AXIS2_PLACEMENT_3D('',#30969,#24602,#24603);
#20829=AXIS2_PLACEMENT_3D('',#30971,#24605,#24606);
#20830=AXIS2_PLACEMENT_3D('',#30973,#24608,#24609);
#20831=AXIS2_PLACEMENT_3D('',#30975,#24611,#24612);
#20832=AXIS2_PLACEMENT_3D('',#30977,#24614,#24615);
#20833=AXIS2_PLACEMENT_3D('',#30978,#24616,#24617);
#20834=AXIS2_PLACEMENT_3D('',#30979,#24618,#24619);
#20835=AXIS2_PLACEMENT_3D('',#30982,#24620,#24621);
#20836=AXIS2_PLACEMENT_3D('',#30986,#24623,#24624);
#20837=AXIS2_PLACEMENT_3D('',#30988,#24626,#24627);
#20838=AXIS2_PLACEMENT_3D('',#30990,#24628,#24629);
#20839=AXIS2_PLACEMENT_3D('',#30993,#24631,#24632);
#20840=AXIS2_PLACEMENT_3D('',#30994,#24633,#24634);
#20841=AXIS2_PLACEMENT_3D('',#31000,#24638,#24639);
#20842=AXIS2_PLACEMENT_3D('',#31002,#24640,#24641);
#20843=AXIS2_PLACEMENT_3D('',#31005,#24643,#24644);
#20844=AXIS2_PLACEMENT_3D('',#31006,#24645,#24646);
#20845=AXIS2_PLACEMENT_3D('',#31008,#24647,#24648);
#20846=AXIS2_PLACEMENT_3D('',#31011,#24650,#24651);
#20847=AXIS2_PLACEMENT_3D('',#31012,#24652,#24653);
#20848=AXIS2_PLACEMENT_3D('',#31018,#24657,#24658);
#20849=AXIS2_PLACEMENT_3D('',#31020,#24659,#24660);
#20850=AXIS2_PLACEMENT_3D('',#31023,#24662,#24663);
#20851=AXIS2_PLACEMENT_3D('',#31024,#24664,#24665);
#20852=AXIS2_PLACEMENT_3D('',#31026,#24666,#24667);
#20853=AXIS2_PLACEMENT_3D('',#31029,#24669,#24670);
#20854=AXIS2_PLACEMENT_3D('',#31030,#24671,#24672);
#20855=AXIS2_PLACEMENT_3D('',#31032,#24673,#24674);
#20856=AXIS2_PLACEMENT_3D('',#31035,#24676,#24677);
#20857=AXIS2_PLACEMENT_3D('',#31036,#24678,#24679);
#20858=AXIS2_PLACEMENT_3D('',#31042,#24683,#24684);
#20859=AXIS2_PLACEMENT_3D('',#31044,#24685,#24686);
#20860=AXIS2_PLACEMENT_3D('',#31047,#24688,#24689);
#20861=AXIS2_PLACEMENT_3D('',#31048,#24690,#24691);
#20862=AXIS2_PLACEMENT_3D('',#31054,#24695,#24696);
#20863=AXIS2_PLACEMENT_3D('',#31056,#24697,#24698);
#20864=AXIS2_PLACEMENT_3D('',#31059,#24700,#24701);
#20865=AXIS2_PLACEMENT_3D('',#31060,#24702,#24703);
#20866=AXIS2_PLACEMENT_3D('',#31062,#24704,#24705);
#20867=AXIS2_PLACEMENT_3D('',#31065,#24707,#24708);
#20868=AXIS2_PLACEMENT_3D('',#31066,#24709,#24710);
#20869=AXIS2_PLACEMENT_3D('',#31068,#24711,#24712);
#20870=AXIS2_PLACEMENT_3D('',#31071,#24714,#24715);
#20871=AXIS2_PLACEMENT_3D('',#31072,#24716,#24717);
#20872=AXIS2_PLACEMENT_3D('',#31078,#24721,#24722);
#20873=AXIS2_PLACEMENT_3D('',#31080,#24723,#24724);
#20874=AXIS2_PLACEMENT_3D('',#31083,#24726,#24727);
#20875=AXIS2_PLACEMENT_3D('',#31084,#24728,#24729);
#20876=AXIS2_PLACEMENT_3D('',#31086,#24730,#24731);
#20877=AXIS2_PLACEMENT_3D('',#31089,#24733,#24734);
#20878=AXIS2_PLACEMENT_3D('',#31090,#24735,#24736);
#20879=AXIS2_PLACEMENT_3D('',#31096,#24740,#24741);
#20880=AXIS2_PLACEMENT_3D('',#31097,#24742,#24743);
#20881=AXIS2_PLACEMENT_3D('',#31098,#24744,#24745);
#20882=AXIS2_PLACEMENT_3D('',#31099,#24746,#24747);
#20883=AXIS2_PLACEMENT_3D('',#31100,#24748,#24749);
#20884=AXIS2_PLACEMENT_3D('',#31101,#24750,#24751);
#20885=AXIS2_PLACEMENT_3D('',#31102,#24752,#24753);
#20886=AXIS2_PLACEMENT_3D('',#31105,#24754,#24755);
#20887=AXIS2_PLACEMENT_3D('',#31109,#24757,#24758);
#20888=AXIS2_PLACEMENT_3D('',#31111,#24760,#24761);
#20889=AXIS2_PLACEMENT_3D('',#31113,#24762,#24763);
#20890=AXIS2_PLACEMENT_3D('',#31116,#24765,#24766);
#20891=AXIS2_PLACEMENT_3D('',#31117,#24767,#24768);
#20892=AXIS2_PLACEMENT_3D('',#31119,#24769,#24770);
#20893=AXIS2_PLACEMENT_3D('',#31122,#24772,#24773);
#20894=AXIS2_PLACEMENT_3D('',#31123,#24774,#24775);
#20895=AXIS2_PLACEMENT_3D('',#31129,#24779,#24780);
#20896=AXIS2_PLACEMENT_3D('',#31132,#24781,#24782);
#20897=AXIS2_PLACEMENT_3D('',#31136,#24784,#24785);
#20898=AXIS2_PLACEMENT_3D('',#31138,#24787,#24788);
#20899=AXIS2_PLACEMENT_3D('',#31140,#24789,#24790);
#20900=AXIS2_PLACEMENT_3D('',#31143,#24792,#24793);
#20901=AXIS2_PLACEMENT_3D('',#31144,#24794,#24795);
#20902=AXIS2_PLACEMENT_3D('',#31146,#24796,#24797);
#20903=AXIS2_PLACEMENT_3D('',#31149,#24799,#24800);
#20904=AXIS2_PLACEMENT_3D('',#31150,#24801,#24802);
#20905=AXIS2_PLACEMENT_3D('',#31156,#24806,#24807);
#20906=AXIS2_PLACEMENT_3D('',#31159,#24808,#24809);
#20907=AXIS2_PLACEMENT_3D('',#31163,#24811,#24812);
#20908=AXIS2_PLACEMENT_3D('',#31165,#24814,#24815);
#20909=AXIS2_PLACEMENT_3D('',#31167,#24816,#24817);
#20910=AXIS2_PLACEMENT_3D('',#31170,#24819,#24820);
#20911=AXIS2_PLACEMENT_3D('',#31171,#24821,#24822);
#20912=AXIS2_PLACEMENT_3D('',#31173,#24823,#24824);
#20913=AXIS2_PLACEMENT_3D('',#31176,#24826,#24827);
#20914=AXIS2_PLACEMENT_3D('',#31177,#24828,#24829);
#20915=AXIS2_PLACEMENT_3D('',#31183,#24833,#24834);
#20916=AXIS2_PLACEMENT_3D('',#31186,#24835,#24836);
#20917=AXIS2_PLACEMENT_3D('',#31190,#24838,#24839);
#20918=AXIS2_PLACEMENT_3D('',#31192,#24841,#24842);
#20919=AXIS2_PLACEMENT_3D('',#31194,#24843,#24844);
#20920=AXIS2_PLACEMENT_3D('',#31197,#24846,#24847);
#20921=AXIS2_PLACEMENT_3D('',#31198,#24848,#24849);
#20922=AXIS2_PLACEMENT_3D('',#31200,#24850,#24851);
#20923=AXIS2_PLACEMENT_3D('',#31203,#24853,#24854);
#20924=AXIS2_PLACEMENT_3D('',#31204,#24855,#24856);
#20925=AXIS2_PLACEMENT_3D('',#31210,#24860,#24861);
#20926=AXIS2_PLACEMENT_3D('',#31213,#24862,#24863);
#20927=AXIS2_PLACEMENT_3D('',#31217,#24865,#24866);
#20928=AXIS2_PLACEMENT_3D('',#31219,#24868,#24869);
#20929=AXIS2_PLACEMENT_3D('',#31221,#24870,#24871);
#20930=AXIS2_PLACEMENT_3D('',#31224,#24873,#24874);
#20931=AXIS2_PLACEMENT_3D('',#31225,#24875,#24876);
#20932=AXIS2_PLACEMENT_3D('',#31227,#24877,#24878);
#20933=AXIS2_PLACEMENT_3D('',#31230,#24880,#24881);
#20934=AXIS2_PLACEMENT_3D('',#31231,#24882,#24883);
#20935=AXIS2_PLACEMENT_3D('',#31237,#24887,#24888);
#20936=AXIS2_PLACEMENT_3D('',#31243,#24892,#24893);
#20937=AXIS2_PLACEMENT_3D('',#31249,#24897,#24898);
#20938=AXIS2_PLACEMENT_3D('',#31255,#24902,#24903);
#20939=AXIS2_PLACEMENT_3D('',#31261,#24907,#24908);
#20940=AXIS2_PLACEMENT_3D('',#31263,#24909,#24910);
#20941=AXIS2_PLACEMENT_3D('',#31266,#24912,#24913);
#20942=AXIS2_PLACEMENT_3D('',#31267,#24914,#24915);
#20943=AXIS2_PLACEMENT_3D('',#31268,#24916,#24917);
#20944=AXIS2_PLACEMENT_3D('',#31269,#24918,#24919);
#20945=AXIS2_PLACEMENT_3D('',#31270,#24920,#24921);
#20946=AXIS2_PLACEMENT_3D('',#31274,#24923,#24924);
#20947=AXIS2_PLACEMENT_3D('',#31277,#24926,#24927);
#20948=AXIS2_PLACEMENT_3D('',#31278,#24928,#24929);
#20949=AXIS2_PLACEMENT_3D('',#31280,#24930,#24931);
#20950=AXIS2_PLACEMENT_3D('',#31282,#24933,#24934);
#20951=AXIS2_PLACEMENT_3D('',#31283,#24935,#24936);
#20952=AXIS2_PLACEMENT_3D('',#31285,#24937,#24938);
#20953=AXIS2_PLACEMENT_3D('',#31287,#24940,#24941);
#20954=AXIS2_PLACEMENT_3D('',#31290,#24943,#24944);
#20955=AXIS2_PLACEMENT_3D('',#31291,#24945,#24946);
#20956=AXIS2_PLACEMENT_3D('',#31293,#24948,#24949);
#20957=AXIS2_PLACEMENT_3D('',#31294,#24950,#24951);
#20958=AXIS2_PLACEMENT_3D('',#31295,#24952,#24953);
#20959=AXIS2_PLACEMENT_3D('',#31299,#24956,#24957);
#20960=AXIS2_PLACEMENT_3D('',#31301,#24958,#24959);
#20961=AXIS2_PLACEMENT_3D('',#31303,#24961,#24962);
#20962=AXIS2_PLACEMENT_3D('',#31305,#24964,#24965);
#20963=AXIS2_PLACEMENT_3D('',#31306,#24966,#24967);
#20964=AXIS2_PLACEMENT_3D('',#31307,#24968,#24969);
#20965=AXIS2_PLACEMENT_3D('',#31308,#24970,#24971);
#20966=AXIS2_PLACEMENT_3D('',#31309,#24972,#24973);
#20967=AXIS2_PLACEMENT_3D('',#31312,#24974,#24975);
#20968=AXIS2_PLACEMENT_3D('',#31316,#24977,#24978);
#20969=AXIS2_PLACEMENT_3D('',#31317,#24979,#24980);
#20970=AXIS2_PLACEMENT_3D('',#31318,#24981,#24982);
#20971=AXIS2_PLACEMENT_3D('',#31320,#24983,#24984);
#20972=AXIS2_PLACEMENT_3D('',#31324,#24986,#24987);
#20973=AXIS2_PLACEMENT_3D('',#31326,#24988,#24989);
#20974=AXIS2_PLACEMENT_3D('',#31327,#24990,#24991);
#20975=AXIS2_PLACEMENT_3D('',#31328,#24992,#24993);
#20976=AXIS2_PLACEMENT_3D('',#31331,#24994,#24995);
#20977=AXIS2_PLACEMENT_3D('',#31335,#24997,#24998);
#20978=AXIS2_PLACEMENT_3D('',#31336,#24999,#25000);
#20979=AXIS2_PLACEMENT_3D('',#31337,#25001,#25002);
#20980=AXIS2_PLACEMENT_3D('',#31339,#25003,#25004);
#20981=AXIS2_PLACEMENT_3D('',#31343,#25006,#25007);
#20982=AXIS2_PLACEMENT_3D('',#31345,#25008,#25009);
#20983=AXIS2_PLACEMENT_3D('',#31346,#25010,#25011);
#20984=AXIS2_PLACEMENT_3D('',#31347,#25012,#25013);
#20985=AXIS2_PLACEMENT_3D('',#31350,#25014,#25015);
#20986=AXIS2_PLACEMENT_3D('',#31354,#25017,#25018);
#20987=AXIS2_PLACEMENT_3D('',#31355,#25019,#25020);
#20988=AXIS2_PLACEMENT_3D('',#31356,#25021,#25022);
#20989=AXIS2_PLACEMENT_3D('',#31358,#25023,#25024);
#20990=AXIS2_PLACEMENT_3D('',#31362,#25026,#25027);
#20991=AXIS2_PLACEMENT_3D('',#31364,#25028,#25029);
#20992=AXIS2_PLACEMENT_3D('',#31365,#25030,#25031);
#20993=AXIS2_PLACEMENT_3D('',#31366,#25032,#25033);
#20994=AXIS2_PLACEMENT_3D('',#31369,#25034,#25035);
#20995=AXIS2_PLACEMENT_3D('',#31373,#25037,#25038);
#20996=AXIS2_PLACEMENT_3D('',#31374,#25039,#25040);
#20997=AXIS2_PLACEMENT_3D('',#31375,#25041,#25042);
#20998=AXIS2_PLACEMENT_3D('',#31377,#25043,#25044);
#20999=AXIS2_PLACEMENT_3D('',#31381,#25046,#25047);
#21000=AXIS2_PLACEMENT_3D('',#31383,#25048,#25049);
#21001=AXIS2_PLACEMENT_3D('',#31384,#25050,#25051);
#21002=AXIS2_PLACEMENT_3D('',#31385,#25052,#25053);
#21003=AXIS2_PLACEMENT_3D('',#31387,#25054,#25055);
#21004=AXIS2_PLACEMENT_3D('',#31389,#25056,#25057);
#21005=AXIS2_PLACEMENT_3D('',#31390,#25058,#25059);
#21006=AXIS2_PLACEMENT_3D('',#31391,#25060,#25061);
#21007=AXIS2_PLACEMENT_3D('',#31393,#25062,#25063);
#21008=AXIS2_PLACEMENT_3D('',#31395,#25064,#25065);
#21009=AXIS2_PLACEMENT_3D('',#31396,#25066,#25067);
#21010=AXIS2_PLACEMENT_3D('',#31397,#25068,#25069);
#21011=AXIS2_PLACEMENT_3D('',#31399,#25070,#25071);
#21012=AXIS2_PLACEMENT_3D('',#31401,#25072,#25073);
#21013=AXIS2_PLACEMENT_3D('',#31402,#25074,#25075);
#21014=AXIS2_PLACEMENT_3D('',#31403,#25076,#25077);
#21015=AXIS2_PLACEMENT_3D('',#31405,#25078,#25079);
#21016=AXIS2_PLACEMENT_3D('',#31407,#25080,#25081);
#21017=AXIS2_PLACEMENT_3D('',#31408,#25082,#25083);
#21018=AXIS2_PLACEMENT_3D('',#31409,#25084,#25085);
#21019=AXIS2_PLACEMENT_3D('',#31412,#25088,#25089);
#21020=AXIS2_PLACEMENT_3D('',#31414,#25091,#25092);
#21021=AXIS2_PLACEMENT_3D('',#31417,#25095,#25096);
#21022=AXIS2_PLACEMENT_3D('',#31419,#25098,#25099);
#21023=AXIS2_PLACEMENT_3D('',#31422,#25102,#25103);
#21024=AXIS2_PLACEMENT_3D('',#31441,#25113,#25114);
#21025=AXIS2_PLACEMENT_3D('',#31443,#25115,#25116);
#21026=AXIS2_PLACEMENT_3D('',#31445,#25117,#25118);
#21027=AXIS2_PLACEMENT_3D('',#31447,#25119,#25120);
#21028=AXIS2_PLACEMENT_3D('',#31448,#25121,#25122);
#21029=AXIS2_PLACEMENT_3D('',#31450,#25124,#25125);
#21030=AXIS2_PLACEMENT_3D('',#31453,#25127,#25128);
#21031=AXIS2_PLACEMENT_3D('',#31455,#25129,#25130);
#21032=AXIS2_PLACEMENT_3D('',#31457,#25131,#25132);
#21033=AXIS2_PLACEMENT_3D('',#31459,#25133,#25134);
#21034=AXIS2_PLACEMENT_3D('',#31461,#25135,#25136);
#21035=AXIS2_PLACEMENT_3D('',#31462,#25137,#25138);
#21036=AXIS2_PLACEMENT_3D('',#31471,#25143,#25144);
#21037=AXIS2_PLACEMENT_3D('',#31477,#25148,#25149);
#21038=AXIS2_PLACEMENT_3D('',#31483,#25153,#25154);
#21039=AXIS2_PLACEMENT_3D('',#31489,#25158,#25159);
#21040=AXIS2_PLACEMENT_3D('',#31495,#25163,#25164);
#21041=AXIS2_PLACEMENT_3D('',#31501,#25168,#25169);
#21042=AXIS2_PLACEMENT_3D('',#31507,#25173,#25174);
#21043=AXIS2_PLACEMENT_3D('',#31510,#25177,#25178);
#21044=AXIS2_PLACEMENT_3D('',#31513,#25181,#25182);
#21045=AXIS2_PLACEMENT_3D('',#31515,#25184,#25185);
#21046=AXIS2_PLACEMENT_3D('',#31517,#25187,#25188);
#21047=AXIS2_PLACEMENT_3D('',#31519,#25190,#25191);
#21048=AXIS2_PLACEMENT_3D('',#31521,#25192,#25193);
#21049=AXIS2_PLACEMENT_3D('',#31522,#25194,#25195);
#21050=AXIS2_PLACEMENT_3D('',#31524,#25197,#25198);
#21051=AXIS2_PLACEMENT_3D('',#31527,#25199,#25200);
#21052=AXIS2_PLACEMENT_3D('',#31530,#25202,#25203);
#21053=AXIS2_PLACEMENT_3D('',#31531,#25204,#25205);
#21054=AXIS2_PLACEMENT_3D('',#31532,#25206,#25207);
#21055=AXIS2_PLACEMENT_3D('',#31534,#25208,#25209);
#21056=AXIS2_PLACEMENT_3D('',#31535,#25210,#25211);
#21057=AXIS2_PLACEMENT_3D('',#31537,#25213,#25214);
#21058=AXIS2_PLACEMENT_3D('',#31540,#25215,#25216);
#21059=AXIS2_PLACEMENT_3D('',#31542,#25218,#25219);
#21060=AXIS2_PLACEMENT_3D('',#31543,#25220,#25221);
#21061=AXIS2_PLACEMENT_3D('',#31545,#25222,#25223);
#21062=AXIS2_PLACEMENT_3D('',#31547,#25225,#25226);
#21063=AXIS2_PLACEMENT_3D('',#31550,#25228,#25229);
#21064=AXIS2_PLACEMENT_3D('',#31551,#25230,#25231);
#21065=AXIS2_PLACEMENT_3D('',#31553,#25232,#25233);
#21066=AXIS2_PLACEMENT_3D('',#31554,#25234,#25235);
#21067=AXIS2_PLACEMENT_3D('',#31556,#25236,#25237);
#21068=AXIS2_PLACEMENT_3D('',#31559,#25239,#25240);
#21069=AXIS2_PLACEMENT_3D('',#31560,#25241,#25242);
#21070=AXIS2_PLACEMENT_3D('',#31562,#25243,#25244);
#21071=AXIS2_PLACEMENT_3D('',#31563,#25245,#25246);
#21072=AXIS2_PLACEMENT_3D('',#31565,#25248,#25249);
#21073=AXIS2_PLACEMENT_3D('',#31568,#25250,#25251);
#21074=AXIS2_PLACEMENT_3D('',#31570,#25253,#25254);
#21075=AXIS2_PLACEMENT_3D('',#31571,#25255,#25256);
#21076=AXIS2_PLACEMENT_3D('',#31574,#25258,#25259);
#21077=AXIS2_PLACEMENT_3D('',#31575,#25260,#25261);
#21078=AXIS2_PLACEMENT_3D('',#31577,#25263,#25264);
#21079=AXIS2_PLACEMENT_3D('',#31579,#25266,#25267);
#21080=AXIS2_PLACEMENT_3D('',#31581,#25269,#25270);
#21081=AXIS2_PLACEMENT_3D('',#31583,#25272,#25273);
#21082=AXIS2_PLACEMENT_3D('',#31585,#25274,#25275);
#21083=AXIS2_PLACEMENT_3D('',#31587,#25277,#25278);
#21084=AXIS2_PLACEMENT_3D('',#31588,#25279,#25280);
#21085=AXIS2_PLACEMENT_3D('',#31590,#25282,#25283);
#21086=AXIS2_PLACEMENT_3D('',#31592,#25285,#25286);
#21087=AXIS2_PLACEMENT_3D('',#31594,#25288,#25289);
#21088=AXIS2_PLACEMENT_3D('',#31595,#25290,#25291);
#21089=AXIS2_PLACEMENT_3D('',#31596,#25292,#25293);
#21090=AXIS2_PLACEMENT_3D('',#31597,#25294,#25295);
#21091=AXIS2_PLACEMENT_3D('',#31600,#25296,#25297);
#21092=AXIS2_PLACEMENT_3D('',#31604,#25299,#25300);
#21093=AXIS2_PLACEMENT_3D('',#31606,#25302,#25303);
#21094=AXIS2_PLACEMENT_3D('',#31608,#25304,#25305);
#21095=AXIS2_PLACEMENT_3D('',#31611,#25307,#25308);
#21096=AXIS2_PLACEMENT_3D('',#31612,#25309,#25310);
#21097=AXIS2_PLACEMENT_3D('',#31614,#25311,#25312);
#21098=AXIS2_PLACEMENT_3D('',#31617,#25314,#25315);
#21099=AXIS2_PLACEMENT_3D('',#31618,#25316,#25317);
#21100=AXIS2_PLACEMENT_3D('',#31624,#25321,#25322);
#21101=AXIS2_PLACEMENT_3D('',#31627,#25323,#25324);
#21102=AXIS2_PLACEMENT_3D('',#31631,#25326,#25327);
#21103=AXIS2_PLACEMENT_3D('',#31633,#25329,#25330);
#21104=AXIS2_PLACEMENT_3D('',#31635,#25331,#25332);
#21105=AXIS2_PLACEMENT_3D('',#31638,#25334,#25335);
#21106=AXIS2_PLACEMENT_3D('',#31639,#25336,#25337);
#21107=AXIS2_PLACEMENT_3D('',#31641,#25338,#25339);
#21108=AXIS2_PLACEMENT_3D('',#31644,#25341,#25342);
#21109=AXIS2_PLACEMENT_3D('',#31645,#25343,#25344);
#21110=AXIS2_PLACEMENT_3D('',#31651,#25348,#25349);
#21111=AXIS2_PLACEMENT_3D('',#31654,#25350,#25351);
#21112=AXIS2_PLACEMENT_3D('',#31658,#25353,#25354);
#21113=AXIS2_PLACEMENT_3D('',#31660,#25356,#25357);
#21114=AXIS2_PLACEMENT_3D('',#31662,#25358,#25359);
#21115=AXIS2_PLACEMENT_3D('',#31665,#25361,#25362);
#21116=AXIS2_PLACEMENT_3D('',#31666,#25363,#25364);
#21117=AXIS2_PLACEMENT_3D('',#31668,#25365,#25366);
#21118=AXIS2_PLACEMENT_3D('',#31671,#25368,#25369);
#21119=AXIS2_PLACEMENT_3D('',#31672,#25370,#25371);
#21120=AXIS2_PLACEMENT_3D('',#31678,#25375,#25376);
#21121=AXIS2_PLACEMENT_3D('',#31681,#25377,#25378);
#21122=AXIS2_PLACEMENT_3D('',#31685,#25380,#25381);
#21123=AXIS2_PLACEMENT_3D('',#31687,#25383,#25384);
#21124=AXIS2_PLACEMENT_3D('',#31689,#25385,#25386);
#21125=AXIS2_PLACEMENT_3D('',#31692,#25388,#25389);
#21126=AXIS2_PLACEMENT_3D('',#31693,#25390,#25391);
#21127=AXIS2_PLACEMENT_3D('',#31695,#25392,#25393);
#21128=AXIS2_PLACEMENT_3D('',#31698,#25395,#25396);
#21129=AXIS2_PLACEMENT_3D('',#31699,#25397,#25398);
#21130=AXIS2_PLACEMENT_3D('',#31705,#25402,#25403);
#21131=AXIS2_PLACEMENT_3D('',#31708,#25404,#25405);
#21132=AXIS2_PLACEMENT_3D('',#31712,#25407,#25408);
#21133=AXIS2_PLACEMENT_3D('',#31714,#25410,#25411);
#21134=AXIS2_PLACEMENT_3D('',#31716,#25412,#25413);
#21135=AXIS2_PLACEMENT_3D('',#31719,#25415,#25416);
#21136=AXIS2_PLACEMENT_3D('',#31720,#25417,#25418);
#21137=AXIS2_PLACEMENT_3D('',#31722,#25419,#25420);
#21138=AXIS2_PLACEMENT_3D('',#31725,#25422,#25423);
#21139=AXIS2_PLACEMENT_3D('',#31726,#25424,#25425);
#21140=AXIS2_PLACEMENT_3D('',#31732,#25429,#25430);
#21141=AXIS2_PLACEMENT_3D('',#31738,#25434,#25435);
#21142=AXIS2_PLACEMENT_3D('',#31744,#25439,#25440);
#21143=AXIS2_PLACEMENT_3D('',#31750,#25444,#25445);
#21144=AXIS2_PLACEMENT_3D('',#31756,#25449,#25450);
#21145=AXIS2_PLACEMENT_3D('',#31758,#25451,#25452);
#21146=AXIS2_PLACEMENT_3D('',#31761,#25454,#25455);
#21147=AXIS2_PLACEMENT_3D('',#31762,#25456,#25457);
#21148=AXIS2_PLACEMENT_3D('',#31763,#25458,#25459);
#21149=AXIS2_PLACEMENT_3D('',#31764,#25460,#25461);
#21150=AXIS2_PLACEMENT_3D('',#31765,#25462,#25463);
#21151=AXIS2_PLACEMENT_3D('',#31769,#25465,#25466);
#21152=AXIS2_PLACEMENT_3D('',#31772,#25468,#25469);
#21153=AXIS2_PLACEMENT_3D('',#31773,#25470,#25471);
#21154=AXIS2_PLACEMENT_3D('',#31775,#25472,#25473);
#21155=AXIS2_PLACEMENT_3D('',#31777,#25475,#25476);
#21156=AXIS2_PLACEMENT_3D('',#31778,#25477,#25478);
#21157=AXIS2_PLACEMENT_3D('',#31780,#25479,#25480);
#21158=AXIS2_PLACEMENT_3D('',#31782,#25482,#25483);
#21159=AXIS2_PLACEMENT_3D('',#31785,#25485,#25486);
#21160=AXIS2_PLACEMENT_3D('',#31786,#25487,#25488);
#21161=AXIS2_PLACEMENT_3D('',#31788,#25490,#25491);
#21162=AXIS2_PLACEMENT_3D('',#31789,#25492,#25493);
#21163=AXIS2_PLACEMENT_3D('',#31790,#25494,#25495);
#21164=AXIS2_PLACEMENT_3D('',#31794,#25498,#25499);
#21165=AXIS2_PLACEMENT_3D('',#31796,#25500,#25501);
#21166=AXIS2_PLACEMENT_3D('',#31798,#25503,#25504);
#21167=AXIS2_PLACEMENT_3D('',#31800,#25506,#25507);
#21168=AXIS2_PLACEMENT_3D('',#31801,#25508,#25509);
#21169=AXIS2_PLACEMENT_3D('',#31802,#25510,#25511);
#21170=AXIS2_PLACEMENT_3D('',#31803,#25512,#25513);
#21171=AXIS2_PLACEMENT_3D('',#31804,#25514,#25515);
#21172=AXIS2_PLACEMENT_3D('',#31809,#25517,#25518);
#21173=AXIS2_PLACEMENT_3D('',#31811,#25519,#25520);
#21174=AXIS2_PLACEMENT_3D('',#31816,#25521,#25522);
#21175=AXIS2_PLACEMENT_3D('',#31817,#25523,#25524);
#21176=AXIS2_PLACEMENT_3D('',#31818,#25525,#25526);
#21177=AXIS2_PLACEMENT_3D('',#31823,#25527,#25528);
#21178=AXIS2_PLACEMENT_3D('',#31824,#25529,#25530);
#21179=AXIS2_PLACEMENT_3D('',#31826,#25531,#25532);
#21180=AXIS2_PLACEMENT_3D('',#31829,#25534,#25535);
#21181=AXIS2_PLACEMENT_3D('',#31830,#25536,#25537);
#21182=AXIS2_PLACEMENT_3D('',#31832,#25538,#25539);
#21183=AXIS2_PLACEMENT_3D('',#31833,#25540,#25541);
#21184=AXIS2_PLACEMENT_3D('',#31835,#25542,#25543);
#21185=AXIS2_PLACEMENT_3D('',#31836,#25544,#25545);
#21186=AXIS2_PLACEMENT_3D('',#31842,#25549,#25550);
#21187=AXIS2_PLACEMENT_3D('',#31843,#25551,#25552);
#21188=AXIS2_PLACEMENT_3D('',#31845,#25554,#25555);
#21189=AXIS2_PLACEMENT_3D('',#31846,#25556,#25557);
#21190=AXIS2_PLACEMENT_3D('',#31850,#25559,#25560);
#21191=AXIS2_PLACEMENT_3D('',#31851,#25561,#25562);
#21192=AXIS2_PLACEMENT_3D('',#31852,#25563,#25564);
#21193=AXIS2_PLACEMENT_3D('',#31855,#25566,#25567);
#21194=AXIS2_PLACEMENT_3D('',#31856,#25568,#25569);
#21195=AXIS2_PLACEMENT_3D('',#31857,#25570,#25571);
#21196=AXIS2_PLACEMENT_3D('',#31858,#25572,#25573);
#21197=AXIS2_PLACEMENT_3D('',#31859,#25574,#25575);
#21198=AXIS2_PLACEMENT_3D('',#31868,#25580,#25581);
#21199=AXIS2_PLACEMENT_3D('',#31877,#25586,#25587);
#21200=AXIS2_PLACEMENT_3D('',#31883,#25591,#25592);
#21201=AXIS2_PLACEMENT_3D('',#31889,#25596,#25597);
#21202=AXIS2_PLACEMENT_3D('',#31895,#25601,#25602);
#21203=AXIS2_PLACEMENT_3D('',#31906,#25608,#25609);
#21204=AXIS2_PLACEMENT_3D('',#31912,#25613,#25614);
#21205=AXIS2_PLACEMENT_3D('',#31916,#25617,#25618);
#21206=AXIS2_PLACEMENT_3D('',#31922,#25622,#25623);
#21207=AXIS2_PLACEMENT_3D('',#31926,#25626,#25627);
#21208=AXIS2_PLACEMENT_3D('',#31928,#25629,#25630);
#21209=AXIS2_PLACEMENT_3D('',#31930,#25632,#25633);
#21210=AXIS2_PLACEMENT_3D('',#31932,#25634,#25635);
#21211=AXIS2_PLACEMENT_3D('',#31934,#25637,#25638);
#21212=AXIS2_PLACEMENT_3D('',#31938,#25641,#25642);
#21213=AXIS2_PLACEMENT_3D('',#31942,#25645,#25646);
#21214=AXIS2_PLACEMENT_3D('',#31944,#25648,#25649);
#21215=AXIS2_PLACEMENT_3D('',#31945,#25650,#25651);
#21216=AXIS2_PLACEMENT_3D('',#31946,#25652,#25653);
#21217=AXIS2_PLACEMENT_3D('',#31948,#25654,#25655);
#21218=AXIS2_PLACEMENT_3D('',#31951,#25657,#25658);
#21219=AXIS2_PLACEMENT_3D('',#31952,#25659,#25660);
#21220=AXIS2_PLACEMENT_3D('',#31954,#25661,#25662);
#21221=AXIS2_PLACEMENT_3D('',#31957,#25664,#25665);
#21222=AXIS2_PLACEMENT_3D('',#31958,#25666,#25667);
#21223=AXIS2_PLACEMENT_3D('',#31960,#25668,#25669);
#21224=AXIS2_PLACEMENT_3D('',#31963,#25671,#25672);
#21225=AXIS2_PLACEMENT_3D('',#31964,#25673,#25674);
#21226=AXIS2_PLACEMENT_3D('',#31966,#25675,#25676);
#21227=AXIS2_PLACEMENT_3D('',#31969,#25678,#25679);
#21228=AXIS2_PLACEMENT_3D('',#31970,#25680,#25681);
#21229=AXIS2_PLACEMENT_3D('',#31972,#25682,#25683);
#21230=AXIS2_PLACEMENT_3D('',#31975,#25685,#25686);
#21231=AXIS2_PLACEMENT_3D('',#31976,#25687,#25688);
#21232=AXIS2_PLACEMENT_3D('',#31978,#25689,#25690);
#21233=AXIS2_PLACEMENT_3D('',#31981,#25692,#25693);
#21234=AXIS2_PLACEMENT_3D('',#31982,#25694,#25695);
#21235=AXIS2_PLACEMENT_3D('',#31984,#25696,#25697);
#21236=AXIS2_PLACEMENT_3D('',#31987,#25699,#25700);
#21237=AXIS2_PLACEMENT_3D('',#31988,#25701,#25702);
#21238=AXIS2_PLACEMENT_3D('',#31990,#25703,#25704);
#21239=AXIS2_PLACEMENT_3D('',#31993,#25706,#25707);
#21240=AXIS2_PLACEMENT_3D('',#31994,#25708,#25709);
#21241=AXIS2_PLACEMENT_3D('',#31996,#25710,#25711);
#21242=AXIS2_PLACEMENT_3D('',#31999,#25713,#25714);
#21243=AXIS2_PLACEMENT_3D('',#32000,#25715,#25716);
#21244=AXIS2_PLACEMENT_3D('',#32002,#25717,#25718);
#21245=AXIS2_PLACEMENT_3D('',#32005,#25720,#25721);
#21246=AXIS2_PLACEMENT_3D('',#32006,#25722,#25723);
#21247=AXIS2_PLACEMENT_3D('',#32015,#25728,#25729);
#21248=AXIS2_PLACEMENT_3D('',#32021,#25733,#25734);
#21249=AXIS2_PLACEMENT_3D('',#32030,#25739,#25740);
#21250=AXIS2_PLACEMENT_3D('',#32033,#25743,#25744);
#21251=AXIS2_PLACEMENT_3D('',#32042,#25749,#25750);
#21252=AXIS2_PLACEMENT_3D('',#32048,#25754,#25755);
#21253=AXIS2_PLACEMENT_3D('',#32051,#25758,#25759);
#21254=AXIS2_PLACEMENT_3D('',#32053,#25760,#25761);
#21255=AXIS2_PLACEMENT_3D('',#32055,#25762,#25763);
#21256=AXIS2_PLACEMENT_3D('',#32057,#25765,#25766);
#21257=AXIS2_PLACEMENT_3D('',#32063,#25770,#25771);
#21258=AXIS2_PLACEMENT_3D('',#32066,#25774,#25775);
#21259=AXIS2_PLACEMENT_3D('',#32067,#25776,#25777);
#21260=AXIS2_PLACEMENT_3D('',#32068,#25778,#25779);
#21261=AXIS2_PLACEMENT_3D('',#32069,#25780,#25781);
#21262=AXIS2_PLACEMENT_3D('',#32078,#25786,#25787);
#21263=AXIS2_PLACEMENT_3D('',#32084,#25791,#25792);
#21264=AXIS2_PLACEMENT_3D('',#32089,#25794,#25795);
#21265=AXIS2_PLACEMENT_3D('',#32092,#25797,#25798);
#21266=AXIS2_PLACEMENT_3D('',#32093,#25799,#25800);
#21267=AXIS2_PLACEMENT_3D('',#32096,#25803,#25804);
#21268=AXIS2_PLACEMENT_3D('',#32102,#25808,#25809);
#21269=AXIS2_PLACEMENT_3D('',#32106,#25812,#25813);
#21270=AXIS2_PLACEMENT_3D('',#32110,#25816,#25817);
#21271=AXIS2_PLACEMENT_3D('',#32112,#25819,#25820);
#21272=AXIS2_PLACEMENT_3D('',#32113,#25821,#25822);
#21273=AXIS2_PLACEMENT_3D('',#32114,#25823,#25824);
#21274=AXIS2_PLACEMENT_3D('',#32117,#25825,#25826);
#21275=AXIS2_PLACEMENT_3D('',#32121,#25828,#25829);
#21276=AXIS2_PLACEMENT_3D('',#32123,#25831,#25832);
#21277=AXIS2_PLACEMENT_3D('',#32125,#25833,#25834);
#21278=AXIS2_PLACEMENT_3D('',#32128,#25836,#25837);
#21279=AXIS2_PLACEMENT_3D('',#32129,#25838,#25839);
#21280=AXIS2_PLACEMENT_3D('',#32131,#25840,#25841);
#21281=AXIS2_PLACEMENT_3D('',#32134,#25843,#25844);
#21282=AXIS2_PLACEMENT_3D('',#32135,#25845,#25846);
#21283=AXIS2_PLACEMENT_3D('',#32141,#25850,#25851);
#21284=AXIS2_PLACEMENT_3D('',#32144,#25852,#25853);
#21285=AXIS2_PLACEMENT_3D('',#32148,#25855,#25856);
#21286=AXIS2_PLACEMENT_3D('',#32150,#25858,#25859);
#21287=AXIS2_PLACEMENT_3D('',#32152,#25860,#25861);
#21288=AXIS2_PLACEMENT_3D('',#32155,#25863,#25864);
#21289=AXIS2_PLACEMENT_3D('',#32156,#25865,#25866);
#21290=AXIS2_PLACEMENT_3D('',#32158,#25867,#25868);
#21291=AXIS2_PLACEMENT_3D('',#32161,#25870,#25871);
#21292=AXIS2_PLACEMENT_3D('',#32162,#25872,#25873);
#21293=AXIS2_PLACEMENT_3D('',#32168,#25877,#25878);
#21294=AXIS2_PLACEMENT_3D('',#32171,#25879,#25880);
#21295=AXIS2_PLACEMENT_3D('',#32175,#25882,#25883);
#21296=AXIS2_PLACEMENT_3D('',#32177,#25885,#25886);
#21297=AXIS2_PLACEMENT_3D('',#32179,#25887,#25888);
#21298=AXIS2_PLACEMENT_3D('',#32182,#25890,#25891);
#21299=AXIS2_PLACEMENT_3D('',#32183,#25892,#25893);
#21300=AXIS2_PLACEMENT_3D('',#32185,#25894,#25895);
#21301=AXIS2_PLACEMENT_3D('',#32188,#25897,#25898);
#21302=AXIS2_PLACEMENT_3D('',#32189,#25899,#25900);
#21303=AXIS2_PLACEMENT_3D('',#32195,#25904,#25905);
#21304=AXIS2_PLACEMENT_3D('',#32198,#25906,#25907);
#21305=AXIS2_PLACEMENT_3D('',#32202,#25909,#25910);
#21306=AXIS2_PLACEMENT_3D('',#32204,#25912,#25913);
#21307=AXIS2_PLACEMENT_3D('',#32206,#25914,#25915);
#21308=AXIS2_PLACEMENT_3D('',#32209,#25917,#25918);
#21309=AXIS2_PLACEMENT_3D('',#32210,#25919,#25920);
#21310=AXIS2_PLACEMENT_3D('',#32212,#25921,#25922);
#21311=AXIS2_PLACEMENT_3D('',#32215,#25924,#25925);
#21312=AXIS2_PLACEMENT_3D('',#32216,#25926,#25927);
#21313=AXIS2_PLACEMENT_3D('',#32222,#25931,#25932);
#21314=AXIS2_PLACEMENT_3D('',#32225,#25933,#25934);
#21315=AXIS2_PLACEMENT_3D('',#32229,#25936,#25937);
#21316=AXIS2_PLACEMENT_3D('',#32231,#25939,#25940);
#21317=AXIS2_PLACEMENT_3D('',#32233,#25941,#25942);
#21318=AXIS2_PLACEMENT_3D('',#32236,#25944,#25945);
#21319=AXIS2_PLACEMENT_3D('',#32237,#25946,#25947);
#21320=AXIS2_PLACEMENT_3D('',#32239,#25948,#25949);
#21321=AXIS2_PLACEMENT_3D('',#32242,#25951,#25952);
#21322=AXIS2_PLACEMENT_3D('',#32243,#25953,#25954);
#21323=AXIS2_PLACEMENT_3D('',#32249,#25958,#25959);
#21324=AXIS2_PLACEMENT_3D('',#32255,#25963,#25964);
#21325=AXIS2_PLACEMENT_3D('',#32261,#25968,#25969);
#21326=AXIS2_PLACEMENT_3D('',#32267,#25973,#25974);
#21327=AXIS2_PLACEMENT_3D('',#32273,#25978,#25979);
#21328=AXIS2_PLACEMENT_3D('',#32275,#25980,#25981);
#21329=AXIS2_PLACEMENT_3D('',#32278,#25983,#25984);
#21330=AXIS2_PLACEMENT_3D('',#32279,#25985,#25986);
#21331=AXIS2_PLACEMENT_3D('',#32280,#25987,#25988);
#21332=AXIS2_PLACEMENT_3D('',#32281,#25989,#25990);
#21333=AXIS2_PLACEMENT_3D('',#32282,#25991,#25992);
#21334=AXIS2_PLACEMENT_3D('',#32286,#25994,#25995);
#21335=AXIS2_PLACEMENT_3D('',#32289,#25997,#25998);
#21336=AXIS2_PLACEMENT_3D('',#32290,#25999,#26000);
#21337=AXIS2_PLACEMENT_3D('',#32292,#26001,#26002);
#21338=AXIS2_PLACEMENT_3D('',#32294,#26004,#26005);
#21339=AXIS2_PLACEMENT_3D('',#32295,#26006,#26007);
#21340=AXIS2_PLACEMENT_3D('',#32297,#26008,#26009);
#21341=AXIS2_PLACEMENT_3D('',#32299,#26011,#26012);
#21342=AXIS2_PLACEMENT_3D('',#32302,#26014,#26015);
#21343=AXIS2_PLACEMENT_3D('',#32303,#26016,#26017);
#21344=AXIS2_PLACEMENT_3D('',#32305,#26019,#26020);
#21345=AXIS2_PLACEMENT_3D('',#32306,#26021,#26022);
#21346=AXIS2_PLACEMENT_3D('',#32307,#26023,#26024);
#21347=AXIS2_PLACEMENT_3D('',#32311,#26026,#26027);
#21348=AXIS2_PLACEMENT_3D('',#32313,#26029,#26030);
#21349=AXIS2_PLACEMENT_3D('',#32315,#26032,#26033);
#21350=AXIS2_PLACEMENT_3D('',#32316,#26034,#26035);
#21351=AXIS2_PLACEMENT_3D('',#32317,#26036,#26037);
#21352=AXIS2_PLACEMENT_3D('',#32319,#26039,#26040);
#21353=AXIS2_PLACEMENT_3D('',#32320,#26041,#26042);
#21354=AXIS2_PLACEMENT_3D('',#32321,#26043,#26044);
#21355=AXIS2_PLACEMENT_3D('',#32323,#26045,#26046);
#21356=AXIS2_PLACEMENT_3D('',#32325,#26047,#26048);
#21357=AXIS2_PLACEMENT_3D('',#32326,#26049,#26050);
#21358=AXIS2_PLACEMENT_3D('',#32329,#26052,#26053);
#21359=AXIS2_PLACEMENT_3D('',#32330,#26054,#26055);
#21360=AXIS2_PLACEMENT_3D('',#32332,#26056,#26057);
#21361=AXIS2_PLACEMENT_3D('',#32334,#26059,#26060);
#21362=AXIS2_PLACEMENT_3D('',#32335,#26061,#26062);
#21363=AXIS2_PLACEMENT_3D('',#32336,#26063,#26064);
#21364=AXIS2_PLACEMENT_3D('',#32345,#26069,#26070);
#21365=AXIS2_PLACEMENT_3D('',#32351,#26074,#26075);
#21366=AXIS2_PLACEMENT_3D('',#32355,#26077,#26078);
#21367=AXIS2_PLACEMENT_3D('',#32361,#26082,#26083);
#21368=AXIS2_PLACEMENT_3D('',#32366,#26086,#26087);
#21369=AXIS2_PLACEMENT_3D('',#32367,#26088,#26089);
#21370=AXIS2_PLACEMENT_3D('',#32374,#26094,#26095);
#21371=AXIS2_PLACEMENT_3D('',#32375,#26096,#26097);
#21372=AXIS2_PLACEMENT_3D('',#32377,#26099,#26100);
#21373=AXIS2_PLACEMENT_3D('',#32379,#26102,#26103);
#21374=AXIS2_PLACEMENT_3D('',#32380,#26104,#26105);
#21375=AXIS2_PLACEMENT_3D('',#32381,#26106,#26107);
#21376=AXIS2_PLACEMENT_3D('',#32386,#26109,#26110);
#21377=AXIS2_PLACEMENT_3D('',#32389,#26112,#26113);
#21378=AXIS2_PLACEMENT_3D('',#32390,#26114,#26115);
#21379=AXIS2_PLACEMENT_3D('',#32395,#26117,#26118);
#21380=AXIS2_PLACEMENT_3D('',#32398,#26120,#26121);
#21381=AXIS2_PLACEMENT_3D('',#32399,#26122,#26123);
#21382=AXIS2_PLACEMENT_3D('',#32404,#26125,#26126);
#21383=AXIS2_PLACEMENT_3D('',#32407,#26128,#26129);
#21384=AXIS2_PLACEMENT_3D('',#32408,#26130,#26131);
#21385=AXIS2_PLACEMENT_3D('',#32413,#26133,#26134);
#21386=AXIS2_PLACEMENT_3D('',#32416,#26136,#26137);
#21387=AXIS2_PLACEMENT_3D('',#32417,#26138,#26139);
#21388=AXIS2_PLACEMENT_3D('',#32422,#26141,#26142);
#21389=AXIS2_PLACEMENT_3D('',#32425,#26144,#26145);
#21390=AXIS2_PLACEMENT_3D('',#32426,#26146,#26147);
#21391=AXIS2_PLACEMENT_3D('',#32431,#26149,#26150);
#21392=AXIS2_PLACEMENT_3D('',#32434,#26152,#26153);
#21393=AXIS2_PLACEMENT_3D('',#32435,#26154,#26155);
#21394=AXIS2_PLACEMENT_3D('',#32440,#26157,#26158);
#21395=AXIS2_PLACEMENT_3D('',#32443,#26160,#26161);
#21396=AXIS2_PLACEMENT_3D('',#32444,#26162,#26163);
#21397=AXIS2_PLACEMENT_3D('',#32449,#26165,#26166);
#21398=AXIS2_PLACEMENT_3D('',#32452,#26168,#26169);
#21399=AXIS2_PLACEMENT_3D('',#32453,#26170,#26171);
#21400=AXIS2_PLACEMENT_3D('',#32458,#26173,#26174);
#21401=AXIS2_PLACEMENT_3D('',#32461,#26176,#26177);
#21402=AXIS2_PLACEMENT_3D('',#32462,#26178,#26179);
#21403=AXIS2_PLACEMENT_3D('',#32467,#26181,#26182);
#21404=AXIS2_PLACEMENT_3D('',#32470,#26184,#26185);
#21405=AXIS2_PLACEMENT_3D('',#32471,#26186,#26187);
#21406=AXIS2_PLACEMENT_3D('',#32476,#26189,#26190);
#21407=AXIS2_PLACEMENT_3D('',#32479,#26192,#26193);
#21408=AXIS2_PLACEMENT_3D('',#32480,#26194,#26195);
#21409=AXIS2_PLACEMENT_3D('',#32485,#26197,#26198);
#21410=AXIS2_PLACEMENT_3D('',#32488,#26200,#26201);
#21411=AXIS2_PLACEMENT_3D('',#32489,#26202,#26203);
#21412=AXIS2_PLACEMENT_3D('',#32494,#26205,#26206);
#21413=AXIS2_PLACEMENT_3D('',#32497,#26208,#26209);
#21414=AXIS2_PLACEMENT_3D('',#32498,#26210,#26211);
#21415=AXIS2_PLACEMENT_3D('',#32503,#26213,#26214);
#21416=AXIS2_PLACEMENT_3D('',#32506,#26216,#26217);
#21417=AXIS2_PLACEMENT_3D('',#32507,#26218,#26219);
#21418=AXIS2_PLACEMENT_3D('',#32512,#26221,#26222);
#21419=AXIS2_PLACEMENT_3D('',#32515,#26224,#26225);
#21420=AXIS2_PLACEMENT_3D('',#32516,#26226,#26227);
#21421=AXIS2_PLACEMENT_3D('',#32521,#26229,#26230);
#21422=AXIS2_PLACEMENT_3D('',#32524,#26232,#26233);
#21423=AXIS2_PLACEMENT_3D('',#32525,#26234,#26235);
#21424=AXIS2_PLACEMENT_3D('',#32530,#26237,#26238);
#21425=AXIS2_PLACEMENT_3D('',#32533,#26240,#26241);
#21426=AXIS2_PLACEMENT_3D('',#32534,#26242,#26243);
#21427=AXIS2_PLACEMENT_3D('',#32539,#26245,#26246);
#21428=AXIS2_PLACEMENT_3D('',#32542,#26248,#26249);
#21429=AXIS2_PLACEMENT_3D('',#32543,#26250,#26251);
#21430=AXIS2_PLACEMENT_3D('',#32548,#26253,#26254);
#21431=AXIS2_PLACEMENT_3D('',#32551,#26256,#26257);
#21432=AXIS2_PLACEMENT_3D('',#32552,#26258,#26259);
#21433=AXIS2_PLACEMENT_3D('',#32557,#26261,#26262);
#21434=AXIS2_PLACEMENT_3D('',#32560,#26264,#26265);
#21435=AXIS2_PLACEMENT_3D('',#32561,#26266,#26267);
#21436=AXIS2_PLACEMENT_3D('',#32566,#26269,#26270);
#21437=AXIS2_PLACEMENT_3D('',#32569,#26272,#26273);
#21438=AXIS2_PLACEMENT_3D('',#32570,#26274,#26275);
#21439=AXIS2_PLACEMENT_3D('',#32575,#26277,#26278);
#21440=AXIS2_PLACEMENT_3D('',#32578,#26280,#26281);
#21441=AXIS2_PLACEMENT_3D('',#32579,#26282,#26283);
#21442=AXIS2_PLACEMENT_3D('',#32584,#26285,#26286);
#21443=AXIS2_PLACEMENT_3D('',#32587,#26288,#26289);
#21444=AXIS2_PLACEMENT_3D('',#32588,#26290,#26291);
#21445=AXIS2_PLACEMENT_3D('',#32593,#26293,#26294);
#21446=AXIS2_PLACEMENT_3D('',#32596,#26296,#26297);
#21447=AXIS2_PLACEMENT_3D('',#32597,#26298,#26299);
#21448=AXIS2_PLACEMENT_3D('',#32602,#26301,#26302);
#21449=AXIS2_PLACEMENT_3D('',#32605,#26304,#26305);
#21450=AXIS2_PLACEMENT_3D('',#32606,#26306,#26307);
#21451=AXIS2_PLACEMENT_3D('',#32611,#26309,#26310);
#21452=AXIS2_PLACEMENT_3D('',#32614,#26312,#26313);
#21453=AXIS2_PLACEMENT_3D('',#32615,#26314,#26315);
#21454=AXIS2_PLACEMENT_3D('',#32620,#26317,#26318);
#21455=AXIS2_PLACEMENT_3D('',#32623,#26320,#26321);
#21456=AXIS2_PLACEMENT_3D('',#32624,#26322,#26323);
#21457=AXIS2_PLACEMENT_3D('',#32629,#26325,#26326);
#21458=AXIS2_PLACEMENT_3D('',#32632,#26328,#26329);
#21459=AXIS2_PLACEMENT_3D('',#32633,#26330,#26331);
#21460=AXIS2_PLACEMENT_3D('',#32638,#26333,#26334);
#21461=AXIS2_PLACEMENT_3D('',#32641,#26336,#26337);
#21462=AXIS2_PLACEMENT_3D('',#32642,#26338,#26339);
#21463=AXIS2_PLACEMENT_3D('',#32647,#26341,#26342);
#21464=AXIS2_PLACEMENT_3D('',#32650,#26344,#26345);
#21465=AXIS2_PLACEMENT_3D('',#32651,#26346,#26347);
#21466=AXIS2_PLACEMENT_3D('',#32656,#26349,#26350);
#21467=AXIS2_PLACEMENT_3D('',#32659,#26352,#26353);
#21468=AXIS2_PLACEMENT_3D('',#32660,#26354,#26355);
#21469=AXIS2_PLACEMENT_3D('',#32665,#26357,#26358);
#21470=AXIS2_PLACEMENT_3D('',#32668,#26360,#26361);
#21471=AXIS2_PLACEMENT_3D('',#32669,#26362,#26363);
#21472=AXIS2_PLACEMENT_3D('',#32674,#26365,#26366);
#21473=AXIS2_PLACEMENT_3D('',#32677,#26368,#26369);
#21474=AXIS2_PLACEMENT_3D('',#32678,#26370,#26371);
#21475=AXIS2_PLACEMENT_3D('',#32683,#26373,#26374);
#21476=AXIS2_PLACEMENT_3D('',#32686,#26376,#26377);
#21477=AXIS2_PLACEMENT_3D('',#32687,#26378,#26379);
#21478=AXIS2_PLACEMENT_3D('',#32692,#26381,#26382);
#21479=AXIS2_PLACEMENT_3D('',#32695,#26384,#26385);
#21480=AXIS2_PLACEMENT_3D('',#32696,#26386,#26387);
#21481=AXIS2_PLACEMENT_3D('',#32701,#26389,#26390);
#21482=AXIS2_PLACEMENT_3D('',#32704,#26392,#26393);
#21483=AXIS2_PLACEMENT_3D('',#32705,#26394,#26395);
#21484=AXIS2_PLACEMENT_3D('',#32710,#26397,#26398);
#21485=AXIS2_PLACEMENT_3D('',#32713,#26400,#26401);
#21486=AXIS2_PLACEMENT_3D('',#32714,#26402,#26403);
#21487=AXIS2_PLACEMENT_3D('',#32719,#26405,#26406);
#21488=AXIS2_PLACEMENT_3D('',#32722,#26408,#26409);
#21489=AXIS2_PLACEMENT_3D('',#32723,#26410,#26411);
#21490=AXIS2_PLACEMENT_3D('',#32728,#26413,#26414);
#21491=AXIS2_PLACEMENT_3D('',#32731,#26416,#26417);
#21492=AXIS2_PLACEMENT_3D('',#32732,#26418,#26419);
#21493=AXIS2_PLACEMENT_3D('',#32737,#26421,#26422);
#21494=AXIS2_PLACEMENT_3D('',#32740,#26424,#26425);
#21495=AXIS2_PLACEMENT_3D('',#32741,#26426,#26427);
#21496=AXIS2_PLACEMENT_3D('',#32746,#26429,#26430);
#21497=AXIS2_PLACEMENT_3D('',#32749,#26432,#26433);
#21498=AXIS2_PLACEMENT_3D('',#32750,#26434,#26435);
#21499=AXIS2_PLACEMENT_3D('',#32755,#26437,#26438);
#21500=AXIS2_PLACEMENT_3D('',#32758,#26440,#26441);
#21501=AXIS2_PLACEMENT_3D('',#32759,#26442,#26443);
#21502=AXIS2_PLACEMENT_3D('',#32764,#26445,#26446);
#21503=AXIS2_PLACEMENT_3D('',#32767,#26448,#26449);
#21504=AXIS2_PLACEMENT_3D('',#32768,#26450,#26451);
#21505=AXIS2_PLACEMENT_3D('',#32773,#26453,#26454);
#21506=AXIS2_PLACEMENT_3D('',#32776,#26456,#26457);
#21507=AXIS2_PLACEMENT_3D('',#32777,#26458,#26459);
#21508=AXIS2_PLACEMENT_3D('',#32779,#26460,#26461);
#21509=AXIS2_PLACEMENT_3D('',#32781,#26462,#26463);
#21510=AXIS2_PLACEMENT_3D('',#32782,#26464,#26465);
#21511=AXIS2_PLACEMENT_3D('',#32783,#26466,#26467);
#21512=AXIS2_PLACEMENT_3D('',#32784,#26468,#26469);
#21513=AXIS2_PLACEMENT_3D('',#32785,#26470,#26471);
#21514=AXIS2_PLACEMENT_3D('',#32786,#26472,#26473);
#21515=AXIS2_PLACEMENT_3D('',#32787,#26474,#26475);
#21516=AXIS2_PLACEMENT_3D('',#32788,#26476,#26477);
#21517=AXIS2_PLACEMENT_3D('',#32789,#26478,#26479);
#21518=AXIS2_PLACEMENT_3D('',#32790,#26480,#26481);
#21519=AXIS2_PLACEMENT_3D('',#32791,#26482,#26483);
#21520=AXIS2_PLACEMENT_3D('',#32792,#26484,#26485);
#21521=AXIS2_PLACEMENT_3D('',#32793,#26486,#26487);
#21522=AXIS2_PLACEMENT_3D('',#32794,#26488,#26489);
#21523=AXIS2_PLACEMENT_3D('',#32795,#26490,#26491);
#21524=AXIS2_PLACEMENT_3D('',#32796,#26492,#26493);
#21525=AXIS2_PLACEMENT_3D('',#32797,#26494,#26495);
#21526=AXIS2_PLACEMENT_3D('',#32798,#26496,#26497);
#21527=AXIS2_PLACEMENT_3D('',#32799,#26498,#26499);
#21528=AXIS2_PLACEMENT_3D('',#32800,#26500,#26501);
#21529=AXIS2_PLACEMENT_3D('',#32801,#26502,#26503);
#21530=AXIS2_PLACEMENT_3D('',#32802,#26504,#26505);
#21531=AXIS2_PLACEMENT_3D('',#32803,#26506,#26507);
#21532=AXIS2_PLACEMENT_3D('',#32804,#26508,#26509);
#21533=AXIS2_PLACEMENT_3D('',#32805,#26510,#26511);
#21534=AXIS2_PLACEMENT_3D('',#32806,#26512,#26513);
#21535=AXIS2_PLACEMENT_3D('',#32807,#26514,#26515);
#21536=AXIS2_PLACEMENT_3D('',#32808,#26516,#26517);
#21537=AXIS2_PLACEMENT_3D('',#32809,#26518,#26519);
#21538=AXIS2_PLACEMENT_3D('',#32810,#26520,#26521);
#21539=AXIS2_PLACEMENT_3D('',#32811,#26522,#26523);
#21540=AXIS2_PLACEMENT_3D('',#32812,#26524,#26525);
#21541=AXIS2_PLACEMENT_3D('',#32813,#26526,#26527);
#21542=AXIS2_PLACEMENT_3D('',#32814,#26528,#26529);
#21543=AXIS2_PLACEMENT_3D('',#32815,#26530,#26531);
#21544=AXIS2_PLACEMENT_3D('',#32816,#26532,#26533);
#21545=AXIS2_PLACEMENT_3D('',#32817,#26534,#26535);
#21546=AXIS2_PLACEMENT_3D('',#32818,#26536,#26537);
#21547=AXIS2_PLACEMENT_3D('',#32819,#26538,#26539);
#21548=AXIS2_PLACEMENT_3D('',#32820,#26540,#26541);
#21549=AXIS2_PLACEMENT_3D('',#32821,#26542,#26543);
#21550=AXIS2_PLACEMENT_3D('',#32822,#26544,#26545);
#21551=AXIS2_PLACEMENT_3D('',#32823,#26546,#26547);
#21552=AXIS2_PLACEMENT_3D('',#32824,#26548,#26549);
#21553=AXIS2_PLACEMENT_3D('',#32825,#26550,#26551);
#21554=AXIS2_PLACEMENT_3D('',#32827,#26552,#26553);
#21555=AXIS2_PLACEMENT_3D('',#32828,#26554,#26555);
#21556=AXIS2_PLACEMENT_3D('',#32830,#26556,#26557);
#21557=AXIS2_PLACEMENT_3D('',#32832,#26559,#26560);
#21558=AXIS2_PLACEMENT_3D('',#32835,#26562,#26563);
#21559=AXIS2_PLACEMENT_3D('',#32836,#26564,#26565);
#21560=AXIS2_PLACEMENT_3D('',#32837,#26566,#26567);
#21561=AXIS2_PLACEMENT_3D('',#32838,#26568,#26569);
#21562=AXIS2_PLACEMENT_3D('',#32839,#26570,#26571);
#21563=AXIS2_PLACEMENT_3D('',#32840,#26572,#26573);
#21564=AXIS2_PLACEMENT_3D('',#32841,#26574,#26575);
#21565=AXIS2_PLACEMENT_3D('',#32842,#26576,#26577);
#21566=AXIS2_PLACEMENT_3D('',#32843,#26578,#26579);
#21567=AXIS2_PLACEMENT_3D('',#32844,#26580,#26581);
#21568=AXIS2_PLACEMENT_3D('',#32845,#26582,#26583);
#21569=AXIS2_PLACEMENT_3D('',#32846,#26584,#26585);
#21570=AXIS2_PLACEMENT_3D('',#32847,#26586,#26587);
#21571=AXIS2_PLACEMENT_3D('',#32848,#26588,#26589);
#21572=AXIS2_PLACEMENT_3D('',#32849,#26590,#26591);
#21573=AXIS2_PLACEMENT_3D('',#32850,#26592,#26593);
#21574=AXIS2_PLACEMENT_3D('',#32851,#26594,#26595);
#21575=AXIS2_PLACEMENT_3D('',#32852,#26596,#26597);
#21576=AXIS2_PLACEMENT_3D('',#32853,#26598,#26599);
#21577=AXIS2_PLACEMENT_3D('',#32854,#26600,#26601);
#21578=AXIS2_PLACEMENT_3D('',#32855,#26602,#26603);
#21579=AXIS2_PLACEMENT_3D('',#32856,#26604,#26605);
#21580=AXIS2_PLACEMENT_3D('',#32857,#26606,#26607);
#21581=AXIS2_PLACEMENT_3D('',#32858,#26608,#26609);
#21582=AXIS2_PLACEMENT_3D('',#32859,#26610,#26611);
#21583=AXIS2_PLACEMENT_3D('',#32860,#26612,#26613);
#21584=AXIS2_PLACEMENT_3D('',#32861,#26614,#26615);
#21585=AXIS2_PLACEMENT_3D('',#32862,#26616,#26617);
#21586=AXIS2_PLACEMENT_3D('',#32863,#26618,#26619);
#21587=AXIS2_PLACEMENT_3D('',#32864,#26620,#26621);
#21588=AXIS2_PLACEMENT_3D('',#32865,#26622,#26623);
#21589=AXIS2_PLACEMENT_3D('',#32866,#26624,#26625);
#21590=AXIS2_PLACEMENT_3D('',#32867,#26626,#26627);
#21591=AXIS2_PLACEMENT_3D('',#32868,#26628,#26629);
#21592=AXIS2_PLACEMENT_3D('',#32869,#26630,#26631);
#21593=AXIS2_PLACEMENT_3D('',#32870,#26632,#26633);
#21594=AXIS2_PLACEMENT_3D('',#32871,#26634,#26635);
#21595=AXIS2_PLACEMENT_3D('',#32872,#26636,#26637);
#21596=AXIS2_PLACEMENT_3D('',#32873,#26638,#26639);
#21597=AXIS2_PLACEMENT_3D('',#32874,#26640,#26641);
#21598=AXIS2_PLACEMENT_3D('',#32875,#26642,#26643);
#21599=AXIS2_PLACEMENT_3D('',#32876,#26644,#26645);
#21600=AXIS2_PLACEMENT_3D('',#32877,#26646,#26647);
#21601=AXIS2_PLACEMENT_3D('',#32878,#26648,#26649);
#21602=AXIS2_PLACEMENT_3D('',#32879,#26650,#26651);
#21603=AXIS2_PLACEMENT_3D('',#32880,#26652,#26653);
#21604=AXIS2_PLACEMENT_3D('',#32881,#26654,#26655);
#21605=AXIS2_PLACEMENT_3D('',#32882,#26656,#26657);
#21606=AXIS2_PLACEMENT_3D('',#32883,#26658,#26659);
#21607=AXIS2_PLACEMENT_3D('',#32884,#26660,#26661);
#21608=AXIS2_PLACEMENT_3D('',#32885,#26662,#26663);
#21609=AXIS2_PLACEMENT_3D('',#32886,#26664,#26665);
#21610=AXIS2_PLACEMENT_3D('',#32887,#26666,#26667);
#21611=AXIS2_PLACEMENT_3D('',#32888,#26668,#26669);
#21612=AXIS2_PLACEMENT_3D('',#32889,#26670,#26671);
#21613=AXIS2_PLACEMENT_3D('',#32890,#26672,#26673);
#21614=AXIS2_PLACEMENT_3D('',#32891,#26674,#26675);
#21615=AXIS2_PLACEMENT_3D('',#32892,#26676,#26677);
#21616=AXIS2_PLACEMENT_3D('',#32893,#26678,#26679);
#21617=AXIS2_PLACEMENT_3D('',#32894,#26680,#26681);
#21618=AXIS2_PLACEMENT_3D('',#32895,#26682,#26683);
#21619=AXIS2_PLACEMENT_3D('',#32896,#26684,#26685);
#21620=AXIS2_PLACEMENT_3D('',#32897,#26686,#26687);
#21621=AXIS2_PLACEMENT_3D('',#32898,#26688,#26689);
#21622=AXIS2_PLACEMENT_3D('',#32899,#26690,#26691);
#21623=AXIS2_PLACEMENT_3D('',#32900,#26692,#26693);
#21624=AXIS2_PLACEMENT_3D('',#32901,#26694,#26695);
#21625=AXIS2_PLACEMENT_3D('',#32902,#26696,#26697);
#21626=AXIS2_PLACEMENT_3D('',#32903,#26698,#26699);
#21627=AXIS2_PLACEMENT_3D('',#32904,#26700,#26701);
#21628=AXIS2_PLACEMENT_3D('',#32905,#26702,#26703);
#21629=AXIS2_PLACEMENT_3D('',#32906,#26704,#26705);
#21630=AXIS2_PLACEMENT_3D('',#32907,#26706,#26707);
#21631=AXIS2_PLACEMENT_3D('',#32908,#26708,#26709);
#21632=AXIS2_PLACEMENT_3D('',#32909,#26710,#26711);
#21633=AXIS2_PLACEMENT_3D('',#32910,#26712,#26713);
#21634=AXIS2_PLACEMENT_3D('',#32911,#26714,#26715);
#21635=AXIS2_PLACEMENT_3D('',#32912,#26716,#26717);
#21636=AXIS2_PLACEMENT_3D('',#32913,#26718,#26719);
#21637=AXIS2_PLACEMENT_3D('',#32914,#26720,#26721);
#21638=AXIS2_PLACEMENT_3D('',#32915,#26722,#26723);
#21639=AXIS2_PLACEMENT_3D('',#32916,#26724,#26725);
#21640=AXIS2_PLACEMENT_3D('',#32917,#26726,#26727);
#21641=AXIS2_PLACEMENT_3D('',#32918,#26728,#26729);
#21642=AXIS2_PLACEMENT_3D('',#32919,#26730,#26731);
#21643=AXIS2_PLACEMENT_3D('',#32920,#26732,#26733);
#21644=AXIS2_PLACEMENT_3D('',#32921,#26734,#26735);
#21645=AXIS2_PLACEMENT_3D('',#32922,#26736,#26737);
#21646=AXIS2_PLACEMENT_3D('',#32923,#26738,#26739);
#21647=AXIS2_PLACEMENT_3D('',#32925,#26740,#26741);
#21648=AXIS2_PLACEMENT_3D('',#32926,#26742,#26743);
#21649=AXIS2_PLACEMENT_3D('',#32927,#26744,#26745);
#21650=AXIS2_PLACEMENT_3D('',#32929,#26747,#26748);
#21651=AXIS2_PLACEMENT_3D('',#32930,#26749,#26750);
#21652=AXIS2_PLACEMENT_3D('',#32933,#26751,#26752);
#21653=AXIS2_PLACEMENT_3D('',#32935,#26753,#26754);
#21654=AXIS2_PLACEMENT_3D('',#32936,#26755,#26756);
#21655=AXIS2_PLACEMENT_3D('',#32937,#26757,#26758);
#21656=AXIS2_PLACEMENT_3D('',#32938,#26759,#26760);
#21657=AXIS2_PLACEMENT_3D('',#32941,#26761,#26762);
#21658=AXIS2_PLACEMENT_3D('',#32943,#26764,#26765);
#21659=AXIS2_PLACEMENT_3D('',#32944,#26766,#26767);
#21660=AXIS2_PLACEMENT_3D('',#32946,#26768,#26769);
#21661=AXIS2_PLACEMENT_3D('',#32947,#26770,#26771);
#21662=AXIS2_PLACEMENT_3D('',#32949,#26772,#26773);
#21663=AXIS2_PLACEMENT_3D('',#32950,#26774,#26775);
#21664=AXIS2_PLACEMENT_3D('',#32951,#26776,#26777);
#21665=AXIS2_PLACEMENT_3D('',#32953,#26778,#26779);
#21666=AXIS2_PLACEMENT_3D('',#32954,#26780,#26781);
#21667=AXIS2_PLACEMENT_3D('',#32956,#26783,#26784);
#21668=AXIS2_PLACEMENT_3D('',#32957,#26785,#26786);
#21669=AXIS2_PLACEMENT_3D('',#32960,#26787,#26788);
#21670=AXIS2_PLACEMENT_3D('',#32964,#26790,#26791);
#21671=AXIS2_PLACEMENT_3D('',#32966,#26793,#26794);
#21672=AXIS2_PLACEMENT_3D('',#32968,#26795,#26796);
#21673=AXIS2_PLACEMENT_3D('',#32971,#26798,#26799);
#21674=AXIS2_PLACEMENT_3D('',#32972,#26800,#26801);
#21675=AXIS2_PLACEMENT_3D('',#32974,#26802,#26803);
#21676=AXIS2_PLACEMENT_3D('',#32977,#26805,#26806);
#21677=AXIS2_PLACEMENT_3D('',#32978,#26807,#26808);
#21678=AXIS2_PLACEMENT_3D('',#32984,#26812,#26813);
#21679=AXIS2_PLACEMENT_3D('',#32987,#26814,#26815);
#21680=AXIS2_PLACEMENT_3D('',#32991,#26817,#26818);
#21681=AXIS2_PLACEMENT_3D('',#32993,#26820,#26821);
#21682=AXIS2_PLACEMENT_3D('',#32995,#26822,#26823);
#21683=AXIS2_PLACEMENT_3D('',#32998,#26825,#26826);
#21684=AXIS2_PLACEMENT_3D('',#32999,#26827,#26828);
#21685=AXIS2_PLACEMENT_3D('',#33001,#26829,#26830);
#21686=AXIS2_PLACEMENT_3D('',#33004,#26832,#26833);
#21687=AXIS2_PLACEMENT_3D('',#33005,#26834,#26835);
#21688=AXIS2_PLACEMENT_3D('',#33011,#26839,#26840);
#21689=AXIS2_PLACEMENT_3D('',#33014,#26841,#26842);
#21690=AXIS2_PLACEMENT_3D('',#33018,#26844,#26845);
#21691=AXIS2_PLACEMENT_3D('',#33020,#26847,#26848);
#21692=AXIS2_PLACEMENT_3D('',#33022,#26849,#26850);
#21693=AXIS2_PLACEMENT_3D('',#33025,#26852,#26853);
#21694=AXIS2_PLACEMENT_3D('',#33026,#26854,#26855);
#21695=AXIS2_PLACEMENT_3D('',#33028,#26856,#26857);
#21696=AXIS2_PLACEMENT_3D('',#33031,#26859,#26860);
#21697=AXIS2_PLACEMENT_3D('',#33032,#26861,#26862);
#21698=AXIS2_PLACEMENT_3D('',#33038,#26866,#26867);
#21699=AXIS2_PLACEMENT_3D('',#33041,#26868,#26869);
#21700=AXIS2_PLACEMENT_3D('',#33045,#26871,#26872);
#21701=AXIS2_PLACEMENT_3D('',#33047,#26874,#26875);
#21702=AXIS2_PLACEMENT_3D('',#33049,#26876,#26877);
#21703=AXIS2_PLACEMENT_3D('',#33052,#26879,#26880);
#21704=AXIS2_PLACEMENT_3D('',#33053,#26881,#26882);
#21705=AXIS2_PLACEMENT_3D('',#33055,#26883,#26884);
#21706=AXIS2_PLACEMENT_3D('',#33058,#26886,#26887);
#21707=AXIS2_PLACEMENT_3D('',#33059,#26888,#26889);
#21708=AXIS2_PLACEMENT_3D('',#33065,#26893,#26894);
#21709=AXIS2_PLACEMENT_3D('',#33068,#26895,#26896);
#21710=AXIS2_PLACEMENT_3D('',#33072,#26898,#26899);
#21711=AXIS2_PLACEMENT_3D('',#33074,#26901,#26902);
#21712=AXIS2_PLACEMENT_3D('',#33076,#26903,#26904);
#21713=AXIS2_PLACEMENT_3D('',#33079,#26906,#26907);
#21714=AXIS2_PLACEMENT_3D('',#33080,#26908,#26909);
#21715=AXIS2_PLACEMENT_3D('',#33082,#26910,#26911);
#21716=AXIS2_PLACEMENT_3D('',#33085,#26913,#26914);
#21717=AXIS2_PLACEMENT_3D('',#33086,#26915,#26916);
#21718=AXIS2_PLACEMENT_3D('',#33092,#26920,#26921);
#21719=AXIS2_PLACEMENT_3D('',#33098,#26925,#26926);
#21720=AXIS2_PLACEMENT_3D('',#33104,#26930,#26931);
#21721=AXIS2_PLACEMENT_3D('',#33110,#26935,#26936);
#21722=AXIS2_PLACEMENT_3D('',#33116,#26940,#26941);
#21723=AXIS2_PLACEMENT_3D('',#33118,#26942,#26943);
#21724=AXIS2_PLACEMENT_3D('',#33121,#26945,#26946);
#21725=AXIS2_PLACEMENT_3D('',#33122,#26947,#26948);
#21726=AXIS2_PLACEMENT_3D('',#33123,#26949,#26950);
#21727=AXIS2_PLACEMENT_3D('',#33124,#26951,#26952);
#21728=AXIS2_PLACEMENT_3D('',#33125,#26953,#26954);
#21729=AXIS2_PLACEMENT_3D('',#33129,#26956,#26957);
#21730=AXIS2_PLACEMENT_3D('',#33132,#26959,#26960);
#21731=AXIS2_PLACEMENT_3D('',#33133,#26961,#26962);
#21732=AXIS2_PLACEMENT_3D('',#33135,#26963,#26964);
#21733=AXIS2_PLACEMENT_3D('',#33137,#26966,#26967);
#21734=AXIS2_PLACEMENT_3D('',#33138,#26968,#26969);
#21735=AXIS2_PLACEMENT_3D('',#33140,#26970,#26971);
#21736=AXIS2_PLACEMENT_3D('',#33142,#26973,#26974);
#21737=AXIS2_PLACEMENT_3D('',#33145,#26976,#26977);
#21738=AXIS2_PLACEMENT_3D('',#33146,#26978,#26979);
#21739=AXIS2_PLACEMENT_3D('',#33148,#26981,#26982);
#21740=AXIS2_PLACEMENT_3D('',#33149,#26983,#26984);
#21741=AXIS2_PLACEMENT_3D('',#33150,#26985,#26986);
#21742=AXIS2_PLACEMENT_3D('',#33154,#26989,#26990);
#21743=AXIS2_PLACEMENT_3D('',#33156,#26991,#26992);
#21744=AXIS2_PLACEMENT_3D('',#33158,#26994,#26995);
#21745=AXIS2_PLACEMENT_3D('',#33160,#26997,#26998);
#21746=AXIS2_PLACEMENT_3D('',#33161,#26999,#27000);
#21747=AXIS2_PLACEMENT_3D('',#33162,#27001,#27002);
#21748=AXIS2_PLACEMENT_3D('',#33163,#27003,#27004);
#21749=AXIS2_PLACEMENT_3D('',#33164,#27005,#27006);
#21750=AXIS2_PLACEMENT_3D('',#33173,#27011,#27012);
#21751=AXIS2_PLACEMENT_3D('',#33182,#27017,#27018);
#21752=AXIS2_PLACEMENT_3D('',#33185,#27021,#27022);
#21753=AXIS2_PLACEMENT_3D('',#33187,#27023,#27024);
#21754=AXIS2_PLACEMENT_3D('',#33193,#27028,#27029);
#21755=AXIS2_PLACEMENT_3D('',#33196,#27031,#27032);
#21756=AXIS2_PLACEMENT_3D('',#33197,#27033,#27034);
#21757=AXIS2_PLACEMENT_3D('',#33203,#27038,#27039);
#21758=AXIS2_PLACEMENT_3D('',#33205,#27041,#27042);
#21759=AXIS2_PLACEMENT_3D('',#33207,#27044,#27045);
#21760=AXIS2_PLACEMENT_3D('',#33208,#27046,#27047);
#21761=AXIS2_PLACEMENT_3D('',#33209,#27048,#27049);
#21762=AXIS2_PLACEMENT_3D('',#33214,#27051,#27052);
#21763=AXIS2_PLACEMENT_3D('',#33217,#27054,#27055);
#21764=AXIS2_PLACEMENT_3D('',#33218,#27056,#27057);
#21765=AXIS2_PLACEMENT_3D('',#33224,#27061,#27062);
#21766=AXIS2_PLACEMENT_3D('',#33228,#27064,#27065);
#21767=AXIS2_PLACEMENT_3D('',#33229,#27066,#27067);
#21768=AXIS2_PLACEMENT_3D('',#33230,#27068,#27069);
#21769=AXIS2_PLACEMENT_3D('',#33234,#27071,#27072);
#21770=AXIS2_PLACEMENT_3D('',#33235,#27073,#27074);
#21771=AXIS2_PLACEMENT_3D('',#33236,#27075,#27076);
#21772=AXIS2_PLACEMENT_3D('',#33240,#27078,#27079);
#21773=AXIS2_PLACEMENT_3D('',#33241,#27080,#27081);
#21774=AXIS2_PLACEMENT_3D('',#33242,#27082,#27083);
#21775=AXIS2_PLACEMENT_3D('',#33248,#27087,#27088);
#21776=AXIS2_PLACEMENT_3D('',#33252,#27090,#27091);
#21777=AXIS2_PLACEMENT_3D('',#33253,#27092,#27093);
#21778=AXIS2_PLACEMENT_3D('',#33254,#27094,#27095);
#21779=AXIS2_PLACEMENT_3D('',#33258,#27097,#27098);
#21780=AXIS2_PLACEMENT_3D('',#33259,#27099,#27100);
#21781=AXIS2_PLACEMENT_3D('',#33260,#27101,#27102);
#21782=AXIS2_PLACEMENT_3D('',#33265,#27104,#27105);
#21783=AXIS2_PLACEMENT_3D('',#33268,#27107,#27108);
#21784=AXIS2_PLACEMENT_3D('',#33269,#27109,#27110);
#21785=AXIS2_PLACEMENT_3D('',#33275,#27114,#27115);
#21786=AXIS2_PLACEMENT_3D('',#33277,#27116,#27117);
#21787=AXIS2_PLACEMENT_3D('',#33280,#27119,#27120);
#21788=AXIS2_PLACEMENT_3D('',#33281,#27121,#27122);
#21789=AXIS2_PLACEMENT_3D('',#33283,#27123,#27124);
#21790=AXIS2_PLACEMENT_3D('',#33286,#27126,#27127);
#21791=AXIS2_PLACEMENT_3D('',#33287,#27128,#27129);
#21792=AXIS2_PLACEMENT_3D('',#33289,#27130,#27131);
#21793=AXIS2_PLACEMENT_3D('',#33292,#27133,#27134);
#21794=AXIS2_PLACEMENT_3D('',#33293,#27135,#27136);
#21795=AXIS2_PLACEMENT_3D('',#33299,#27140,#27141);
#21796=AXIS2_PLACEMENT_3D('',#33300,#27142,#27143);
#21797=AXIS2_PLACEMENT_3D('',#33301,#27144,#27145);
#21798=AXIS2_PLACEMENT_3D('',#33302,#27146,#27147);
#21799=AXIS2_PLACEMENT_3D('',#33303,#27148,#27149);
#21800=AXIS2_PLACEMENT_3D('',#33305,#27150,#27151);
#21801=AXIS2_PLACEMENT_3D('',#33307,#27152,#27153);
#21802=AXIS2_PLACEMENT_3D('',#33309,#27154,#27155);
#21803=AXIS2_PLACEMENT_3D('',#33311,#27156,#27157);
#21804=AXIS2_PLACEMENT_3D('',#33328,#27166,#27167);
#21805=AXIS2_PLACEMENT_3D('',#33329,#27168,#27169);
#21806=AXIS2_PLACEMENT_3D('',#33330,#27170,#27171);
#21807=AXIS2_PLACEMENT_3D('',#33333,#27173,#27174);
#21808=AXIS2_PLACEMENT_3D('',#33334,#27175,#27176);
#21809=AXIS2_PLACEMENT_3D('',#33337,#27178,#27179);
#21810=AXIS2_PLACEMENT_3D('',#33338,#27180,#27181);
#21811=AXIS2_PLACEMENT_3D('',#33341,#27183,#27184);
#21812=AXIS2_PLACEMENT_3D('',#33342,#27185,#27186);
#21813=AXIS2_PLACEMENT_3D('',#33345,#27188,#27189);
#21814=AXIS2_PLACEMENT_3D('',#33346,#27190,#27191);
#21815=AXIS2_PLACEMENT_3D('',#33352,#27195,#27196);
#21816=AXIS2_PLACEMENT_3D('',#33356,#27199,#27200);
#21817=AXIS2_PLACEMENT_3D('',#33360,#27203,#27204);
#21818=AXIS2_PLACEMENT_3D('',#33364,#27207,#27208);
#21819=AXIS2_PLACEMENT_3D('',#33368,#27211,#27212);
#21820=AXIS2_PLACEMENT_3D('',#33372,#27215,#27216);
#21821=AXIS2_PLACEMENT_3D('',#33376,#27219,#27220);
#21822=AXIS2_PLACEMENT_3D('',#33378,#27222,#27223);
#21823=AXIS2_PLACEMENT_3D('',#33379,#27224,#27225);
#21824=AXIS2_PLACEMENT_3D('',#33380,#27226,#27227);
#21825=AXIS2_PLACEMENT_3D('',#33383,#27228,#27229);
#21826=AXIS2_PLACEMENT_3D('',#33387,#27231,#27232);
#21827=AXIS2_PLACEMENT_3D('',#33389,#27234,#27235);
#21828=AXIS2_PLACEMENT_3D('',#33391,#27236,#27237);
#21829=AXIS2_PLACEMENT_3D('',#33394,#27239,#27240);
#21830=AXIS2_PLACEMENT_3D('',#33395,#27241,#27242);
#21831=AXIS2_PLACEMENT_3D('',#33397,#27243,#27244);
#21832=AXIS2_PLACEMENT_3D('',#33400,#27246,#27247);
#21833=AXIS2_PLACEMENT_3D('',#33401,#27248,#27249);
#21834=AXIS2_PLACEMENT_3D('',#33407,#27253,#27254);
#21835=AXIS2_PLACEMENT_3D('',#33410,#27255,#27256);
#21836=AXIS2_PLACEMENT_3D('',#33414,#27258,#27259);
#21837=AXIS2_PLACEMENT_3D('',#33416,#27261,#27262);
#21838=AXIS2_PLACEMENT_3D('',#33418,#27263,#27264);
#21839=AXIS2_PLACEMENT_3D('',#33421,#27266,#27267);
#21840=AXIS2_PLACEMENT_3D('',#33422,#27268,#27269);
#21841=AXIS2_PLACEMENT_3D('',#33424,#27270,#27271);
#21842=AXIS2_PLACEMENT_3D('',#33427,#27273,#27274);
#21843=AXIS2_PLACEMENT_3D('',#33428,#27275,#27276);
#21844=AXIS2_PLACEMENT_3D('',#33434,#27280,#27281);
#21845=AXIS2_PLACEMENT_3D('',#33437,#27282,#27283);
#21846=AXIS2_PLACEMENT_3D('',#33441,#27285,#27286);
#21847=AXIS2_PLACEMENT_3D('',#33443,#27288,#27289);
#21848=AXIS2_PLACEMENT_3D('',#33445,#27290,#27291);
#21849=AXIS2_PLACEMENT_3D('',#33448,#27293,#27294);
#21850=AXIS2_PLACEMENT_3D('',#33449,#27295,#27296);
#21851=AXIS2_PLACEMENT_3D('',#33451,#27297,#27298);
#21852=AXIS2_PLACEMENT_3D('',#33454,#27300,#27301);
#21853=AXIS2_PLACEMENT_3D('',#33455,#27302,#27303);
#21854=AXIS2_PLACEMENT_3D('',#33461,#27307,#27308);
#21855=AXIS2_PLACEMENT_3D('',#33464,#27309,#27310);
#21856=AXIS2_PLACEMENT_3D('',#33468,#27312,#27313);
#21857=AXIS2_PLACEMENT_3D('',#33470,#27315,#27316);
#21858=AXIS2_PLACEMENT_3D('',#33472,#27317,#27318);
#21859=AXIS2_PLACEMENT_3D('',#33475,#27320,#27321);
#21860=AXIS2_PLACEMENT_3D('',#33476,#27322,#27323);
#21861=AXIS2_PLACEMENT_3D('',#33478,#27324,#27325);
#21862=AXIS2_PLACEMENT_3D('',#33481,#27327,#27328);
#21863=AXIS2_PLACEMENT_3D('',#33482,#27329,#27330);
#21864=AXIS2_PLACEMENT_3D('',#33488,#27334,#27335);
#21865=AXIS2_PLACEMENT_3D('',#33491,#27336,#27337);
#21866=AXIS2_PLACEMENT_3D('',#33495,#27339,#27340);
#21867=AXIS2_PLACEMENT_3D('',#33497,#27342,#27343);
#21868=AXIS2_PLACEMENT_3D('',#33499,#27344,#27345);
#21869=AXIS2_PLACEMENT_3D('',#33502,#27347,#27348);
#21870=AXIS2_PLACEMENT_3D('',#33503,#27349,#27350);
#21871=AXIS2_PLACEMENT_3D('',#33505,#27351,#27352);
#21872=AXIS2_PLACEMENT_3D('',#33508,#27354,#27355);
#21873=AXIS2_PLACEMENT_3D('',#33509,#27356,#27357);
#21874=AXIS2_PLACEMENT_3D('',#33515,#27361,#27362);
#21875=AXIS2_PLACEMENT_3D('',#33521,#27366,#27367);
#21876=AXIS2_PLACEMENT_3D('',#33527,#27371,#27372);
#21877=AXIS2_PLACEMENT_3D('',#33533,#27376,#27377);
#21878=AXIS2_PLACEMENT_3D('',#33539,#27381,#27382);
#21879=AXIS2_PLACEMENT_3D('',#33541,#27383,#27384);
#21880=AXIS2_PLACEMENT_3D('',#33544,#27386,#27387);
#21881=AXIS2_PLACEMENT_3D('',#33545,#27388,#27389);
#21882=AXIS2_PLACEMENT_3D('',#33546,#27390,#27391);
#21883=AXIS2_PLACEMENT_3D('',#33547,#27392,#27393);
#21884=AXIS2_PLACEMENT_3D('',#33548,#27394,#27395);
#21885=AXIS2_PLACEMENT_3D('',#33552,#27397,#27398);
#21886=AXIS2_PLACEMENT_3D('',#33555,#27400,#27401);
#21887=AXIS2_PLACEMENT_3D('',#33556,#27402,#27403);
#21888=AXIS2_PLACEMENT_3D('',#33558,#27404,#27405);
#21889=AXIS2_PLACEMENT_3D('',#33560,#27407,#27408);
#21890=AXIS2_PLACEMENT_3D('',#33561,#27409,#27410);
#21891=AXIS2_PLACEMENT_3D('',#33563,#27411,#27412);
#21892=AXIS2_PLACEMENT_3D('',#33565,#27414,#27415);
#21893=AXIS2_PLACEMENT_3D('',#33568,#27417,#27418);
#21894=AXIS2_PLACEMENT_3D('',#33569,#27419,#27420);
#21895=AXIS2_PLACEMENT_3D('',#33571,#27422,#27423);
#21896=AXIS2_PLACEMENT_3D('',#33572,#27424,#27425);
#21897=AXIS2_PLACEMENT_3D('',#33573,#27426,#27427);
#21898=AXIS2_PLACEMENT_3D('',#33577,#27429,#27430);
#21899=AXIS2_PLACEMENT_3D('',#33579,#27432,#27433);
#21900=AXIS2_PLACEMENT_3D('',#33581,#27435,#27436);
#21901=AXIS2_PLACEMENT_3D('',#33582,#27437,#27438);
#21902=AXIS2_PLACEMENT_3D('',#33583,#27439,#27440);
#21903=AXIS2_PLACEMENT_3D('',#33585,#27442,#27443);
#21904=AXIS2_PLACEMENT_3D('',#33586,#27444,#27445);
#21905=AXIS2_PLACEMENT_3D('',#33587,#27446,#27447);
#21906=AXIS2_PLACEMENT_3D('',#33596,#27452,#27453);
#21907=AXIS2_PLACEMENT_3D('',#33602,#27457,#27458);
#21908=AXIS2_PLACEMENT_3D('',#33608,#27462,#27463);
#21909=AXIS2_PLACEMENT_3D('',#33611,#27466,#27467);
#21910=AXIS2_PLACEMENT_3D('',#33620,#27472,#27473);
#21911=AXIS2_PLACEMENT_3D('',#33626,#27477,#27478);
#21912=AXIS2_PLACEMENT_3D('',#33632,#27482,#27483);
#21913=AXIS2_PLACEMENT_3D('',#33635,#27486,#27487);
#21914=AXIS2_PLACEMENT_3D('',#33644,#27492,#27493);
#21915=AXIS2_PLACEMENT_3D('',#33650,#27497,#27498);
#21916=AXIS2_PLACEMENT_3D('',#33656,#27502,#27503);
#21917=AXIS2_PLACEMENT_3D('',#33659,#27506,#27507);
#21918=AXIS2_PLACEMENT_3D('',#33668,#27512,#27513);
#21919=AXIS2_PLACEMENT_3D('',#33674,#27517,#27518);
#21920=AXIS2_PLACEMENT_3D('',#33680,#27522,#27523);
#21921=AXIS2_PLACEMENT_3D('',#33683,#27526,#27527);
#21922=AXIS2_PLACEMENT_3D('',#33692,#27532,#27533);
#21923=AXIS2_PLACEMENT_3D('',#33698,#27537,#27538);
#21924=AXIS2_PLACEMENT_3D('',#33704,#27542,#27543);
#21925=AXIS2_PLACEMENT_3D('',#33707,#27546,#27547);
#21926=AXIS2_PLACEMENT_3D('',#33716,#27552,#27553);
#21927=AXIS2_PLACEMENT_3D('',#33722,#27557,#27558);
#21928=AXIS2_PLACEMENT_3D('',#33728,#27562,#27563);
#21929=AXIS2_PLACEMENT_3D('',#33731,#27566,#27567);
#21930=AXIS2_PLACEMENT_3D('',#33740,#27572,#27573);
#21931=AXIS2_PLACEMENT_3D('',#33746,#27577,#27578);
#21932=AXIS2_PLACEMENT_3D('',#33752,#27582,#27583);
#21933=AXIS2_PLACEMENT_3D('',#33762,#27589,#27590);
#21934=AXIS2_PLACEMENT_3D('',#33770,#27595,#27596);
#21935=AXIS2_PLACEMENT_3D('',#33776,#27600,#27601);
#21936=AXIS2_PLACEMENT_3D('',#33796,#27612,#27613);
#21937=AXIS2_PLACEMENT_3D('',#33802,#27617,#27618);
#21938=AXIS2_PLACEMENT_3D('',#33811,#27623,#27624);
#21939=AXIS2_PLACEMENT_3D('',#33814,#27627,#27628);
#21940=AXIS2_PLACEMENT_3D('',#33822,#27633,#27634);
#21941=AXIS2_PLACEMENT_3D('',#33838,#27644,#27645);
#21942=AXIS2_PLACEMENT_3D('',#33844,#27649,#27650);
#21943=AXIS2_PLACEMENT_3D('',#33850,#27654,#27655);
#21944=AXIS2_PLACEMENT_3D('',#33852,#27657,#27658);
#21945=AXIS2_PLACEMENT_3D('',#33861,#27663,#27664);
#21946=AXIS2_PLACEMENT_3D('',#33867,#27668,#27669);
#21947=AXIS2_PLACEMENT_3D('',#33873,#27673,#27674);
#21948=AXIS2_PLACEMENT_3D('',#33880,#27679,#27680);
#21949=AXIS2_PLACEMENT_3D('',#33884,#27684,#27685);
#21950=AXIS2_PLACEMENT_3D('',#33885,#27686,#27687);
#21951=AXIS2_PLACEMENT_3D('',#33887,#27689,#27690);
#21952=AXIS2_PLACEMENT_3D('',#33895,#27695,#27696);
#21953=AXIS2_PLACEMENT_3D('',#33899,#27699,#27700);
#21954=AXIS2_PLACEMENT_3D('',#33906,#27705,#27706);
#21955=AXIS2_PLACEMENT_3D('',#33910,#27709,#27710);
#21956=AXIS2_PLACEMENT_3D('',#33912,#27712,#27713);
#21957=AXIS2_PLACEMENT_3D('',#33914,#27715,#27716);
#21958=AXIS2_PLACEMENT_3D('',#33916,#27718,#27719);
#21959=AXIS2_PLACEMENT_3D('',#33917,#27720,#27721);
#21960=AXIS2_PLACEMENT_3D('',#33918,#27722,#27723);
#21961=AXIS2_PLACEMENT_3D('',#33920,#27724,#27725);
#21962=AXIS2_PLACEMENT_3D('',#33923,#27727,#27728);
#21963=AXIS2_PLACEMENT_3D('',#33924,#27729,#27730);
#21964=AXIS2_PLACEMENT_3D('',#33926,#27731,#27732);
#21965=AXIS2_PLACEMENT_3D('',#33929,#27734,#27735);
#21966=AXIS2_PLACEMENT_3D('',#33930,#27736,#27737);
#21967=AXIS2_PLACEMENT_3D('',#33931,#27738,#27739);
#21968=AXIS2_PLACEMENT_3D('',#33932,#27740,#27741);
#21969=AXIS2_PLACEMENT_3D('',#33933,#27742,#27743);
#21970=AXIS2_PLACEMENT_3D('',#33936,#27744,#27745);
#21971=AXIS2_PLACEMENT_3D('',#33940,#27747,#27748);
#21972=AXIS2_PLACEMENT_3D('',#33942,#27750,#27751);
#21973=AXIS2_PLACEMENT_3D('',#33944,#27752,#27753);
#21974=AXIS2_PLACEMENT_3D('',#33947,#27755,#27756);
#21975=AXIS2_PLACEMENT_3D('',#33948,#27757,#27758);
#21976=AXIS2_PLACEMENT_3D('',#33950,#27759,#27760);
#21977=AXIS2_PLACEMENT_3D('',#33953,#27762,#27763);
#21978=AXIS2_PLACEMENT_3D('',#33954,#27764,#27765);
#21979=AXIS2_PLACEMENT_3D('',#33960,#27769,#27770);
#21980=AXIS2_PLACEMENT_3D('',#33963,#27771,#27772);
#21981=AXIS2_PLACEMENT_3D('',#33967,#27774,#27775);
#21982=AXIS2_PLACEMENT_3D('',#33969,#27777,#27778);
#21983=AXIS2_PLACEMENT_3D('',#33971,#27779,#27780);
#21984=AXIS2_PLACEMENT_3D('',#33974,#27782,#27783);
#21985=AXIS2_PLACEMENT_3D('',#33975,#27784,#27785);
#21986=AXIS2_PLACEMENT_3D('',#33977,#27786,#27787);
#21987=AXIS2_PLACEMENT_3D('',#33980,#27789,#27790);
#21988=AXIS2_PLACEMENT_3D('',#33981,#27791,#27792);
#21989=AXIS2_PLACEMENT_3D('',#33987,#27796,#27797);
#21990=AXIS2_PLACEMENT_3D('',#33990,#27798,#27799);
#21991=AXIS2_PLACEMENT_3D('',#33994,#27801,#27802);
#21992=AXIS2_PLACEMENT_3D('',#33996,#27804,#27805);
#21993=AXIS2_PLACEMENT_3D('',#33998,#27806,#27807);
#21994=AXIS2_PLACEMENT_3D('',#34001,#27809,#27810);
#21995=AXIS2_PLACEMENT_3D('',#34002,#27811,#27812);
#21996=AXIS2_PLACEMENT_3D('',#34004,#27813,#27814);
#21997=AXIS2_PLACEMENT_3D('',#34007,#27816,#27817);
#21998=AXIS2_PLACEMENT_3D('',#34008,#27818,#27819);
#21999=AXIS2_PLACEMENT_3D('',#34014,#27823,#27824);
#22000=AXIS2_PLACEMENT_3D('',#34017,#27825,#27826);
#22001=AXIS2_PLACEMENT_3D('',#34021,#27828,#27829);
#22002=AXIS2_PLACEMENT_3D('',#34023,#27831,#27832);
#22003=AXIS2_PLACEMENT_3D('',#34025,#27833,#27834);
#22004=AXIS2_PLACEMENT_3D('',#34028,#27836,#27837);
#22005=AXIS2_PLACEMENT_3D('',#34029,#27838,#27839);
#22006=AXIS2_PLACEMENT_3D('',#34031,#27840,#27841);
#22007=AXIS2_PLACEMENT_3D('',#34034,#27843,#27844);
#22008=AXIS2_PLACEMENT_3D('',#34035,#27845,#27846);
#22009=AXIS2_PLACEMENT_3D('',#34041,#27850,#27851);
#22010=AXIS2_PLACEMENT_3D('',#34044,#27852,#27853);
#22011=AXIS2_PLACEMENT_3D('',#34048,#27855,#27856);
#22012=AXIS2_PLACEMENT_3D('',#34050,#27858,#27859);
#22013=AXIS2_PLACEMENT_3D('',#34052,#27860,#27861);
#22014=AXIS2_PLACEMENT_3D('',#34055,#27863,#27864);
#22015=AXIS2_PLACEMENT_3D('',#34056,#27865,#27866);
#22016=AXIS2_PLACEMENT_3D('',#34058,#27867,#27868);
#22017=AXIS2_PLACEMENT_3D('',#34061,#27870,#27871);
#22018=AXIS2_PLACEMENT_3D('',#34062,#27872,#27873);
#22019=AXIS2_PLACEMENT_3D('',#34068,#27877,#27878);
#22020=AXIS2_PLACEMENT_3D('',#34074,#27882,#27883);
#22021=AXIS2_PLACEMENT_3D('',#34080,#27887,#27888);
#22022=AXIS2_PLACEMENT_3D('',#34086,#27892,#27893);
#22023=AXIS2_PLACEMENT_3D('',#34092,#27897,#27898);
#22024=AXIS2_PLACEMENT_3D('',#34094,#27899,#27900);
#22025=AXIS2_PLACEMENT_3D('',#34097,#27902,#27903);
#22026=AXIS2_PLACEMENT_3D('',#34098,#27904,#27905);
#22027=AXIS2_PLACEMENT_3D('',#34099,#27906,#27907);
#22028=AXIS2_PLACEMENT_3D('',#34100,#27908,#27909);
#22029=AXIS2_PLACEMENT_3D('',#34101,#27910,#27911);
#22030=AXIS2_PLACEMENT_3D('',#34105,#27913,#27914);
#22031=AXIS2_PLACEMENT_3D('',#34108,#27916,#27917);
#22032=AXIS2_PLACEMENT_3D('',#34109,#27918,#27919);
#22033=AXIS2_PLACEMENT_3D('',#34111,#27920,#27921);
#22034=AXIS2_PLACEMENT_3D('',#34113,#27923,#27924);
#22035=AXIS2_PLACEMENT_3D('',#34114,#27925,#27926);
#22036=AXIS2_PLACEMENT_3D('',#34116,#27927,#27928);
#22037=AXIS2_PLACEMENT_3D('',#34118,#27930,#27931);
#22038=AXIS2_PLACEMENT_3D('',#34121,#27933,#27934);
#22039=AXIS2_PLACEMENT_3D('',#34122,#27935,#27936);
#22040=AXIS2_PLACEMENT_3D('',#34124,#27938,#27939);
#22041=AXIS2_PLACEMENT_3D('',#34125,#27940,#27941);
#22042=AXIS2_PLACEMENT_3D('',#34126,#27942,#27943);
#22043=AXIS2_PLACEMENT_3D('',#34130,#27946,#27947);
#22044=AXIS2_PLACEMENT_3D('',#34132,#27948,#27949);
#22045=AXIS2_PLACEMENT_3D('',#34134,#27951,#27952);
#22046=AXIS2_PLACEMENT_3D('',#34136,#27954,#27955);
#22047=AXIS2_PLACEMENT_3D('',#34137,#27956,#27957);
#22048=AXIS2_PLACEMENT_3D('',#34138,#27958,#27959);
#22049=AXIS2_PLACEMENT_3D('',#34139,#27960,#27961);
#22050=AXIS2_PLACEMENT_3D('',#34140,#27962,#27963);
#22051=AXIS2_PLACEMENT_3D('',#34143,#27964,#27965);
#22052=AXIS2_PLACEMENT_3D('',#34147,#27967,#27968);
#22053=AXIS2_PLACEMENT_3D('',#34149,#27970,#27971);
#22054=AXIS2_PLACEMENT_3D('',#34151,#27972,#27973);
#22055=AXIS2_PLACEMENT_3D('',#34154,#27975,#27976);
#22056=AXIS2_PLACEMENT_3D('',#34155,#27977,#27978);
#22057=AXIS2_PLACEMENT_3D('',#34157,#27979,#27980);
#22058=AXIS2_PLACEMENT_3D('',#34160,#27982,#27983);
#22059=AXIS2_PLACEMENT_3D('',#34161,#27984,#27985);
#22060=AXIS2_PLACEMENT_3D('',#34167,#27989,#27990);
#22061=AXIS2_PLACEMENT_3D('',#34170,#27991,#27992);
#22062=AXIS2_PLACEMENT_3D('',#34174,#27994,#27995);
#22063=AXIS2_PLACEMENT_3D('',#34176,#27997,#27998);
#22064=AXIS2_PLACEMENT_3D('',#34178,#27999,#28000);
#22065=AXIS2_PLACEMENT_3D('',#34181,#28002,#28003);
#22066=AXIS2_PLACEMENT_3D('',#34182,#28004,#28005);
#22067=AXIS2_PLACEMENT_3D('',#34184,#28006,#28007);
#22068=AXIS2_PLACEMENT_3D('',#34187,#28009,#28010);
#22069=AXIS2_PLACEMENT_3D('',#34188,#28011,#28012);
#22070=AXIS2_PLACEMENT_3D('',#34194,#28016,#28017);
#22071=AXIS2_PLACEMENT_3D('',#34197,#28018,#28019);
#22072=AXIS2_PLACEMENT_3D('',#34201,#28021,#28022);
#22073=AXIS2_PLACEMENT_3D('',#34203,#28024,#28025);
#22074=AXIS2_PLACEMENT_3D('',#34205,#28026,#28027);
#22075=AXIS2_PLACEMENT_3D('',#34208,#28029,#28030);
#22076=AXIS2_PLACEMENT_3D('',#34209,#28031,#28032);
#22077=AXIS2_PLACEMENT_3D('',#34211,#28033,#28034);
#22078=AXIS2_PLACEMENT_3D('',#34214,#28036,#28037);
#22079=AXIS2_PLACEMENT_3D('',#34215,#28038,#28039);
#22080=AXIS2_PLACEMENT_3D('',#34221,#28043,#28044);
#22081=AXIS2_PLACEMENT_3D('',#34224,#28045,#28046);
#22082=AXIS2_PLACEMENT_3D('',#34228,#28048,#28049);
#22083=AXIS2_PLACEMENT_3D('',#34230,#28051,#28052);
#22084=AXIS2_PLACEMENT_3D('',#34232,#28053,#28054);
#22085=AXIS2_PLACEMENT_3D('',#34235,#28056,#28057);
#22086=AXIS2_PLACEMENT_3D('',#34236,#28058,#28059);
#22087=AXIS2_PLACEMENT_3D('',#34238,#28060,#28061);
#22088=AXIS2_PLACEMENT_3D('',#34241,#28063,#28064);
#22089=AXIS2_PLACEMENT_3D('',#34242,#28065,#28066);
#22090=AXIS2_PLACEMENT_3D('',#34248,#28070,#28071);
#22091=AXIS2_PLACEMENT_3D('',#34251,#28072,#28073);
#22092=AXIS2_PLACEMENT_3D('',#34255,#28075,#28076);
#22093=AXIS2_PLACEMENT_3D('',#34257,#28078,#28079);
#22094=AXIS2_PLACEMENT_3D('',#34259,#28080,#28081);
#22095=AXIS2_PLACEMENT_3D('',#34262,#28083,#28084);
#22096=AXIS2_PLACEMENT_3D('',#34263,#28085,#28086);
#22097=AXIS2_PLACEMENT_3D('',#34265,#28087,#28088);
#22098=AXIS2_PLACEMENT_3D('',#34268,#28090,#28091);
#22099=AXIS2_PLACEMENT_3D('',#34269,#28092,#28093);
#22100=AXIS2_PLACEMENT_3D('',#34275,#28097,#28098);
#22101=AXIS2_PLACEMENT_3D('',#34281,#28102,#28103);
#22102=AXIS2_PLACEMENT_3D('',#34287,#28107,#28108);
#22103=AXIS2_PLACEMENT_3D('',#34293,#28112,#28113);
#22104=AXIS2_PLACEMENT_3D('',#34299,#28117,#28118);
#22105=AXIS2_PLACEMENT_3D('',#34301,#28119,#28120);
#22106=AXIS2_PLACEMENT_3D('',#34304,#28122,#28123);
#22107=AXIS2_PLACEMENT_3D('',#34305,#28124,#28125);
#22108=AXIS2_PLACEMENT_3D('',#34306,#28126,#28127);
#22109=AXIS2_PLACEMENT_3D('',#34307,#28128,#28129);
#22110=AXIS2_PLACEMENT_3D('',#34308,#28130,#28131);
#22111=AXIS2_PLACEMENT_3D('',#34312,#28133,#28134);
#22112=AXIS2_PLACEMENT_3D('',#34315,#28136,#28137);
#22113=AXIS2_PLACEMENT_3D('',#34316,#28138,#28139);
#22114=AXIS2_PLACEMENT_3D('',#34318,#28140,#28141);
#22115=AXIS2_PLACEMENT_3D('',#34320,#28143,#28144);
#22116=AXIS2_PLACEMENT_3D('',#34321,#28145,#28146);
#22117=AXIS2_PLACEMENT_3D('',#34323,#28147,#28148);
#22118=AXIS2_PLACEMENT_3D('',#34325,#28150,#28151);
#22119=AXIS2_PLACEMENT_3D('',#34328,#28153,#28154);
#22120=AXIS2_PLACEMENT_3D('',#34329,#28155,#28156);
#22121=AXIS2_PLACEMENT_3D('',#34331,#28158,#28159);
#22122=AXIS2_PLACEMENT_3D('',#34332,#28160,#28161);
#22123=AXIS2_PLACEMENT_3D('',#34333,#28162,#28163);
#22124=AXIS2_PLACEMENT_3D('',#34337,#28166,#28167);
#22125=AXIS2_PLACEMENT_3D('',#34339,#28168,#28169);
#22126=AXIS2_PLACEMENT_3D('',#34341,#28171,#28172);
#22127=AXIS2_PLACEMENT_3D('',#34343,#28174,#28175);
#22128=AXIS2_PLACEMENT_3D('',#34344,#28176,#28177);
#22129=AXIS2_PLACEMENT_3D('',#34345,#28178,#28179);
#22130=AXIS2_PLACEMENT_3D('',#34346,#28180,#28181);
#22131=AXIS2_PLACEMENT_3D('',#34347,#28182,#28183);
#22132=AXIS2_PLACEMENT_3D('',#34350,#28184,#28185);
#22133=AXIS2_PLACEMENT_3D('',#34352,#28186,#28187);
#22134=AXIS2_PLACEMENT_3D('',#34353,#28188,#28189);
#22135=AXIS2_PLACEMENT_3D('',#34354,#28190,#28191);
#22136=AXIS2_PLACEMENT_3D('',#34355,#28192,#28193);
#22137=AXIS2_PLACEMENT_3D('',#34358,#28194,#28195);
#22138=AXIS2_PLACEMENT_3D('',#34360,#28197,#28198);
#22139=AXIS2_PLACEMENT_3D('',#34361,#28199,#28200);
#22140=AXIS2_PLACEMENT_3D('',#34363,#28201,#28202);
#22141=AXIS2_PLACEMENT_3D('',#34364,#28203,#28204);
#22142=AXIS2_PLACEMENT_3D('',#34366,#28205,#28206);
#22143=AXIS2_PLACEMENT_3D('',#34367,#28207,#28208);
#22144=AXIS2_PLACEMENT_3D('',#34368,#28209,#28210);
#22145=AXIS2_PLACEMENT_3D('',#34370,#28211,#28212);
#22146=AXIS2_PLACEMENT_3D('',#34371,#28213,#28214);
#22147=AXIS2_PLACEMENT_3D('',#34373,#28216,#28217);
#22148=AXIS2_PLACEMENT_3D('',#34374,#28218,#28219);
#22149=AXIS2_PLACEMENT_3D('',#34383,#28224,#28225);
#22150=AXIS2_PLACEMENT_3D('',#34392,#28230,#28231);
#22151=AXIS2_PLACEMENT_3D('',#34396,#28233,#28234);
#22152=AXIS2_PLACEMENT_3D('',#34397,#28235,#28236);
#22153=AXIS2_PLACEMENT_3D('',#34398,#28237,#28238);
#22154=AXIS2_PLACEMENT_3D('',#34401,#28241,#28242);
#22155=AXIS2_PLACEMENT_3D('',#34407,#28246,#28247);
#22156=AXIS2_PLACEMENT_3D('',#34411,#28250,#28251);
#22157=AXIS2_PLACEMENT_3D('',#34415,#28254,#28255);
#22158=AXIS2_PLACEMENT_3D('',#34417,#28257,#28258);
#22159=AXIS2_PLACEMENT_3D('',#34418,#28259,#28260);
#22160=AXIS2_PLACEMENT_3D('',#34419,#28261,#28262);
#22161=AXIS2_PLACEMENT_3D('',#34422,#28263,#28264);
#22162=AXIS2_PLACEMENT_3D('',#34425,#28266,#28267);
#22163=AXIS2_PLACEMENT_3D('',#34426,#28268,#28269);
#22164=AXIS2_PLACEMENT_3D('',#34427,#28270,#28271);
#22165=AXIS2_PLACEMENT_3D('',#34430,#28273,#28274);
#22166=AXIS2_PLACEMENT_3D('',#34431,#28275,#28276);
#22167=AXIS2_PLACEMENT_3D('',#34432,#28277,#28278);
#22168=AXIS2_PLACEMENT_3D('',#34446,#28279,#28280);
#22169=AXIS2_PLACEMENT_3D('',#34458,#28281,#28282);
#22170=AXIS2_PLACEMENT_3D('',#34459,#28283,#28284);
#22171=AXIS2_PLACEMENT_3D('',#34465,#28285,#28286);
#22172=AXIS2_PLACEMENT_3D('',#34469,#28287,#28288);
#22173=AXIS2_PLACEMENT_3D('',#34483,#28289,#28290);
#22174=AXIS2_PLACEMENT_3D('',#34495,#28291,#28292);
#22175=AXIS2_PLACEMENT_3D('',#34496,#28293,#28294);
#22176=AXIS2_PLACEMENT_3D('',#34502,#28295,#28296);
#22177=AXIS2_PLACEMENT_3D('',#34506,#28297,#28298);
#22178=AXIS2_PLACEMENT_3D('',#34520,#28299,#28300);
#22179=AXIS2_PLACEMENT_3D('',#34532,#28301,#28302);
#22180=AXIS2_PLACEMENT_3D('',#34533,#28303,#28304);
#22181=AXIS2_PLACEMENT_3D('',#34539,#28305,#28306);
#22182=AXIS2_PLACEMENT_3D('',#34541,#28307,#28308);
#22183=AXIS2_PLACEMENT_3D('',#34545,#28309,#28310);
#22184=AXIS2_PLACEMENT_3D('',#34559,#28311,#28312);
#22185=AXIS2_PLACEMENT_3D('',#34571,#28313,#28314);
#22186=AXIS2_PLACEMENT_3D('',#34572,#28315,#28316);
#22187=AXIS2_PLACEMENT_3D('',#34578,#28317,#28318);
#22188=AXIS2_PLACEMENT_3D('',#34582,#28319,#28320);
#22189=AXIS2_PLACEMENT_3D('',#34585,#28321,#28322);
#22190=AXIS2_PLACEMENT_3D('',#34587,#28323,#28324);
#22191=AXIS2_PLACEMENT_3D('',#34588,#28325,#28326);
#22192=AXIS2_PLACEMENT_3D('',#34589,#28327,#28328);
#22193=AXIS2_PLACEMENT_3D('',#34590,#28329,#28330);
#22194=AXIS2_PLACEMENT_3D('',#34592,#28331,#28332);
#22195=AXIS2_PLACEMENT_3D('',#34604,#28333,#28334);
#22196=AXIS2_PLACEMENT_3D('',#34606,#28335,#28336);
#22197=AXIS2_PLACEMENT_3D('',#34618,#28337,#28338);
#22198=AXIS2_PLACEMENT_3D('',#34620,#28339,#28340);
#22199=AXIS2_PLACEMENT_3D('',#34632,#28341,#28342);
#22200=AXIS2_PLACEMENT_3D('',#34634,#28343,#28344);
#22201=AXIS2_PLACEMENT_3D('',#34646,#28345,#28346);
#22202=AXIS2_PLACEMENT_3D('',#34647,#28347,#28348);
#22203=AXIS2_PLACEMENT_3D('',#34649,#28349,#28350);
#22204=AXIS2_PLACEMENT_3D('',#34651,#28352,#28353);
#22205=AXIS2_PLACEMENT_3D('',#34670,#28356,#28357);
#22206=AXIS2_PLACEMENT_3D('',#34674,#28358,#28359);
#22207=AXIS2_PLACEMENT_3D('',#34680,#28361,#28362);
#22208=AXIS2_PLACEMENT_3D('',#34697,#28364,#28365);
#22209=AXIS2_PLACEMENT_3D('',#34703,#28367,#28368);
#22210=AXIS2_PLACEMENT_3D('',#34707,#28369,#28370);
#22211=AXIS2_PLACEMENT_3D('',#34711,#28371,#28372);
#22212=AXIS2_PLACEMENT_3D('',#34717,#28374,#28375);
#22213=AXIS2_PLACEMENT_3D('',#34723,#28377,#28378);
#22214=AXIS2_PLACEMENT_3D('',#34738,#28379,#28380);
#22215=AXIS2_PLACEMENT_3D('',#34755,#28382,#28383);
#22216=AXIS2_PLACEMENT_3D('',#34759,#28384,#28385);
#22217=AXIS2_PLACEMENT_3D('',#34762,#28387,#28388);
#22218=AXIS2_PLACEMENT_3D('',#34764,#28389,#28390);
#22219=AXIS2_PLACEMENT_3D('',#34767,#28392,#28393);
#22220=AXIS2_PLACEMENT_3D('',#34768,#28394,#28395);
#22221=AXIS2_PLACEMENT_3D('',#34769,#28396,#28397);
#22222=AXIS2_PLACEMENT_3D('',#34771,#28399,#28400);
#22223=AXIS2_PLACEMENT_3D('',#34772,#28401,#28402);
#22224=AXIS2_PLACEMENT_3D('',#34773,#28403,#28404);
#22225=AXIS2_PLACEMENT_3D('',#34774,#28405,#28406);
#22226=AXIS2_PLACEMENT_3D('',#34775,#28407,#28408);
#22227=AXIS2_PLACEMENT_3D('',#34776,#28409,#28410);
#22228=AXIS2_PLACEMENT_3D('',#34777,#28411,#28412);
#22229=AXIS2_PLACEMENT_3D('',#34778,#28413,#28414);
#22230=AXIS2_PLACEMENT_3D('',#34779,#28415,#28416);
#22231=AXIS2_PLACEMENT_3D('',#34780,#28417,#28418);
#22232=AXIS2_PLACEMENT_3D('',#34781,#28419,#28420);
#22233=AXIS2_PLACEMENT_3D('',#34782,#28421,#28422);
#22234=AXIS2_PLACEMENT_3D('',#34783,#28423,#28424);
#22235=AXIS2_PLACEMENT_3D('',#34784,#28425,#28426);
#22236=AXIS2_PLACEMENT_3D('',#34785,#28427,#28428);
#22237=AXIS2_PLACEMENT_3D('',#34786,#28429,#28430);
#22238=AXIS2_PLACEMENT_3D('',#34787,#28431,#28432);
#22239=AXIS2_PLACEMENT_3D('',#34788,#28433,#28434);
#22240=AXIS2_PLACEMENT_3D('',#34789,#28435,#28436);
#22241=AXIS2_PLACEMENT_3D('',#34790,#28437,#28438);
#22242=AXIS2_PLACEMENT_3D('',#34791,#28439,#28440);
#22243=AXIS2_PLACEMENT_3D('',#34792,#28441,#28442);
#22244=AXIS2_PLACEMENT_3D('',#34793,#28443,#28444);
#22245=AXIS2_PLACEMENT_3D('',#34794,#28445,#28446);
#22246=AXIS2_PLACEMENT_3D('',#34795,#28447,#28448);
#22247=AXIS2_PLACEMENT_3D('',#34796,#28449,#28450);
#22248=AXIS2_PLACEMENT_3D('',#34797,#28451,#28452);
#22249=AXIS2_PLACEMENT_3D('',#34798,#28453,#28454);
#22250=AXIS2_PLACEMENT_3D('',#34799,#28455,#28456);
#22251=AXIS2_PLACEMENT_3D('',#34800,#28457,#28458);
#22252=AXIS2_PLACEMENT_3D('',#34801,#28459,#28460);
#22253=AXIS2_PLACEMENT_3D('',#34802,#28461,#28462);
#22254=AXIS2_PLACEMENT_3D('',#34803,#28463,#28464);
#22255=AXIS2_PLACEMENT_3D('',#34804,#28465,#28466);
#22256=AXIS2_PLACEMENT_3D('',#34805,#28467,#28468);
#22257=AXIS2_PLACEMENT_3D('',#34806,#28469,#28470);
#22258=DIRECTION('axis',(0.,0.,1.));
#22259=DIRECTION('refdir',(1.,0.,0.));
#22260=DIRECTION('axis',(0.,0.,1.));
#22261=DIRECTION('refdir',(1.,0.,0.));
#22262=DIRECTION('center_axis',(4.55032717710333E-17,-1.,1.51850909121962E-32));
#22263=DIRECTION('ref_axis',(-0.770184521566975,0.,0.637821136948792));
#22264=DIRECTION('center_axis',(-4.55032717710333E-17,1.,-1.51850909121962E-32));
#22265=DIRECTION('ref_axis',(0.637821136949789,2.90229485359357E-17,0.770184521566149));
#22266=DIRECTION('center_axis',(0.637821136948792,2.90229485358903E-17,
0.770184521566975));
#22267=DIRECTION('ref_axis',(0.770184521566975,0.,-0.637821136948792));
#22268=DIRECTION('center_axis',(4.55032717710333E-17,-1.,1.51850909121962E-32));
#22269=DIRECTION('ref_axis',(0.637821136949755,2.90229485359342E-17,0.770184521566178));
#22270=DIRECTION('center_axis',(4.55032717710333E-17,-1.,1.51850909121962E-32));
#22271=DIRECTION('ref_axis',(0.637821136949755,2.90229485359342E-17,0.770184521566178));
#22272=DIRECTION('center_axis',(4.55032717710333E-17,-1.,1.51850909121962E-32));
#22273=DIRECTION('ref_axis',(-0.637821136948792,-2.90229485358903E-17,-0.770184521566975));
#22274=DIRECTION('',(-4.55032717710333E-17,1.,-1.51850909121962E-32));
#22275=DIRECTION('center_axis',(-4.55032717710333E-17,1.,-1.51850909121962E-32));
#22276=DIRECTION('ref_axis',(0.637821136949755,2.90229485359342E-17,0.770184521566178));
#22277=DIRECTION('center_axis',(-4.55032717710333E-17,1.,-1.51850909121962E-32));
#22278=DIRECTION('ref_axis',(0.637821136949755,2.90229485359342E-17,0.770184521566178));
#22279=DIRECTION('center_axis',(4.55032717710333E-17,-1.,1.51850909121962E-32));
#22280=DIRECTION('ref_axis',(-0.637821136948792,-2.90229485358903E-17,-0.770184521566975));
#22281=DIRECTION('center_axis',(4.55032717710333E-17,-1.,1.51850909121962E-32));
#22282=DIRECTION('ref_axis',(-0.637821136948792,-2.90229485358904E-17,-0.770184521566975));
#22283=DIRECTION('center_axis',(4.55032717710333E-17,-1.,1.51850909121962E-32));
#22284=DIRECTION('ref_axis',(-0.770184521566975,-5.42101086242752E-17,0.637821136948792));
#22285=DIRECTION('center_axis',(0.637821136948792,2.90229485358903E-17,
0.770184521566975));
#22286=DIRECTION('ref_axis',(0.770184521566975,3.46944695195361E-17,-0.637821136948792));
#22287=DIRECTION('center_axis',(4.55032717710333E-17,-1.,1.51850909121962E-32));
#22288=DIRECTION('ref_axis',(0.637821136949789,2.90229485359357E-17,0.770184521566149));
#22289=DIRECTION('center_axis',(-4.55032717710333E-17,1.,-1.51850909121962E-32));
#22290=DIRECTION('ref_axis',(0.770184521566975,3.50459155987053E-17,-0.637821136948792));
#22291=DIRECTION('center_axis',(4.55032717710333E-17,-1.,1.51850909121962E-32));
#22292=DIRECTION('ref_axis',(-0.637821136948792,-2.90229485358904E-17,-0.770184521566975));
#22293=DIRECTION('center_axis',(4.55032717710333E-17,-1.,1.51850909121962E-32));
#22294=DIRECTION('ref_axis',(-0.637821136948792,-2.90229485358903E-17,-0.770184521566975));
#22295=DIRECTION('',(4.55032717710333E-17,-1.,1.51850909121962E-32));
#22296=DIRECTION('axis',(0.,0.,1.));
#22297=DIRECTION('refdir',(1.,0.,0.));
#22298=DIRECTION('center_axis',(0.,-1.,0.));
#22299=DIRECTION('ref_axis',(0.959438500558772,0.,0.281918008728665));
#22300=DIRECTION('center_axis',(0.,1.,0.));
#22301=DIRECTION('ref_axis',(0.959438500551132,0.,0.281918008754666));
#22302=DIRECTION('',(0.,-1.,0.));
#22303=DIRECTION('center_axis',(0.,-1.,0.));
#22304=DIRECTION('ref_axis',(0.959438500551132,0.,0.281918008754666));
#22305=DIRECTION('',(0.,1.,0.));
#22306=DIRECTION('center_axis',(0.,-1.,0.));
#22307=DIRECTION('ref_axis',(0.882269183586981,0.,-0.470745247127108));
#22308=DIRECTION('center_axis',(0.,-1.,0.));
#22309=DIRECTION('ref_axis',(0.882269183586837,0.,-0.470745247127378));
#22310=DIRECTION('',(0.,1.,0.));
#22311=DIRECTION('center_axis',(0.,1.,0.));
#22312=DIRECTION('ref_axis',(0.882269183586837,0.,-0.470745247127378));
#22313=DIRECTION('center_axis',(0.,-1.,0.));
#22314=DIRECTION('ref_axis',(0.235571092936033,0.,-0.971857119217081));
#22315=DIRECTION('center_axis',(0.,1.,0.));
#22316=DIRECTION('ref_axis',(0.235571092964656,0.,-0.971857119210143));
#22317=DIRECTION('',(0.,-1.,0.));
#22318=DIRECTION('center_axis',(0.,-1.,0.));
#22319=DIRECTION('ref_axis',(0.235571092964656,0.,-0.971857119210143));
#22320=DIRECTION('center_axis',(-0.528694902398929,0.,-0.848811934516349));
#22321=DIRECTION('ref_axis',(-0.848811934516349,0.,0.528694902398929));
#22322=DIRECTION('',(0.84881193451618,0.,-0.528694902399201));
#22323=DIRECTION('',(0.,1.,0.));
#22324=DIRECTION('',(-0.84881193451618,0.,0.528694902399201));
#22325=DIRECTION('center_axis',(0.,-1.,0.));
#22326=DIRECTION('ref_axis',(0.9880280553808,0.,0.154274306935522));
#22327=DIRECTION('center_axis',(0.,1.,0.));
#22328=DIRECTION('ref_axis',(0.988028055375654,0.,0.154274306968473));
#22329=DIRECTION('',(0.,-1.,0.));
#22330=DIRECTION('center_axis',(0.,-1.,0.));
#22331=DIRECTION('ref_axis',(0.988028055375654,0.,0.154274306968473));
#22332=DIRECTION('',(0.,1.,0.));
#22333=DIRECTION('center_axis',(0.,-1.,0.));
#22334=DIRECTION('ref_axis',(0.813276663802591,0.,-0.581877193327017));
#22335=DIRECTION('center_axis',(0.,-1.,0.));
#22336=DIRECTION('ref_axis',(0.813276663802491,0.,-0.581877193327157));
#22337=DIRECTION('',(0.,1.,0.));
#22338=DIRECTION('center_axis',(0.,1.,0.));
#22339=DIRECTION('ref_axis',(0.813276663802491,0.,-0.581877193327157));
#22340=DIRECTION('center_axis',(0.,-1.,0.));
#22341=DIRECTION('ref_axis',(0.106702940426287,0.,-0.994290944595386));
#22342=DIRECTION('center_axis',(0.,1.,0.));
#22343=DIRECTION('ref_axis',(0.106702940461588,0.,-0.994290944591597));
#22344=DIRECTION('',(0.,-1.,0.));
#22345=DIRECTION('center_axis',(0.,-1.,0.));
#22346=DIRECTION('ref_axis',(0.106702940461588,0.,-0.994290944591597));
#22347=DIRECTION('center_axis',(-0.634964033941301,0.,-0.772541698292714));
#22348=DIRECTION('ref_axis',(-0.772541698292714,0.,0.634964033941301));
#22349=DIRECTION('',(0.772541698292626,0.,-0.634964033941407));
#22350=DIRECTION('',(0.,1.,0.));
#22351=DIRECTION('',(-0.772541698292626,0.,0.634964033941407));
#22352=DIRECTION('center_axis',(0.,-1.,0.));
#22353=DIRECTION('ref_axis',(0.999712176242133,0.,0.0239909289777986));
#22354=DIRECTION('center_axis',(0.,1.,0.));
#22355=DIRECTION('ref_axis',(0.999712176241197,0.,0.0239909290168162));
#22356=DIRECTION('',(0.,-1.,0.));
#22357=DIRECTION('center_axis',(0.,-1.,0.));
#22358=DIRECTION('ref_axis',(0.999712176241197,0.,0.0239909290168162));
#22359=DIRECTION('',(0.,1.,0.));
#22360=DIRECTION('center_axis',(0.,-1.,0.));
#22361=DIRECTION('ref_axis',(0.730368754817649,0.,-0.683053059422266));
#22362=DIRECTION('center_axis',(0.,-1.,0.));
#22363=DIRECTION('ref_axis',(0.730368754817625,0.,-0.683053059422291));
#22364=DIRECTION('',(0.,1.,0.));
#22365=DIRECTION('center_axis',(0.,1.,0.));
#22366=DIRECTION('ref_axis',(0.730368754817625,0.,-0.683053059422291));
#22367=DIRECTION('center_axis',(0.,-1.,0.));
#22368=DIRECTION('ref_axis',(-0.0239909289777984,0.,-0.999712176242133));
#22369=DIRECTION('center_axis',(0.,1.,0.));
#22370=DIRECTION('ref_axis',(-0.023990929016816,0.,-0.999712176241197));
#22371=DIRECTION('',(0.,-1.,0.));
#22372=DIRECTION('center_axis',(0.,-1.,0.));
#22373=DIRECTION('ref_axis',(-0.023990929016816,0.,-0.999712176241197));
#22374=DIRECTION('center_axis',(-0.730368754817648,0.,-0.683053059422266));
#22375=DIRECTION('ref_axis',(-0.683053059422266,0.,0.730368754817648));
#22376=DIRECTION('',(0.683053059422301,0.,-0.730368754817616));
#22377=DIRECTION('',(0.,1.,0.));
#22378=DIRECTION('',(-0.683053059422301,0.,0.730368754817616));
#22379=DIRECTION('center_axis',(0.,-1.,0.));
#22380=DIRECTION('ref_axis',(0.994290944595384,0.,-0.106702940426299));
#22381=DIRECTION('center_axis',(0.,1.,0.));
#22382=DIRECTION('ref_axis',(0.994290944591596,0.,-0.1067029404616));
#22383=DIRECTION('',(0.,-1.,0.));
#22384=DIRECTION('center_axis',(0.,-1.,0.));
#22385=DIRECTION('ref_axis',(0.994290944591596,0.,-0.1067029404616));
#22386=DIRECTION('',(0.,1.,0.));
#22387=DIRECTION('center_axis',(0.,-1.,0.));
#22388=DIRECTION('ref_axis',(0.634964033941301,0.,-0.772541698292714));
#22389=DIRECTION('center_axis',(0.,-1.,0.));
#22390=DIRECTION('ref_axis',(0.63496403394138,0.,-0.772541698292649));
#22391=DIRECTION('',(0.,1.,0.));
#22392=DIRECTION('center_axis',(0.,1.,0.));
#22393=DIRECTION('ref_axis',(0.63496403394138,0.,-0.772541698292649));
#22394=DIRECTION('center_axis',(0.,-1.,0.));
#22395=DIRECTION('ref_axis',(-0.15427430693553,0.,-0.988028055380798));
#22396=DIRECTION('center_axis',(0.,1.,0.));
#22397=DIRECTION('ref_axis',(-0.154274306968481,0.,-0.988028055375653));
#22398=DIRECTION('',(0.,-1.,0.));
#22399=DIRECTION('center_axis',(0.,-1.,0.));
#22400=DIRECTION('ref_axis',(-0.154274306968481,0.,-0.988028055375653));
#22401=DIRECTION('center_axis',(-0.813276663802591,0.,-0.581877193327018));
#22402=DIRECTION('ref_axis',(-0.581877193327018,0.,0.813276663802591));
#22403=DIRECTION('',(0.581877193327206,0.,-0.813276663802456));
#22404=DIRECTION('',(0.,1.,0.));
#22405=DIRECTION('',(-0.581877193327206,0.,0.813276663802456));
#22406=DIRECTION('center_axis',(0.,-1.,0.));
#22407=DIRECTION('ref_axis',(0.971857119217081,0.,-0.235571092936033));
#22408=DIRECTION('center_axis',(0.,1.,0.));
#22409=DIRECTION('ref_axis',(0.971857119210143,0.,-0.235571092964656));
#22410=DIRECTION('',(0.,-1.,0.));
#22411=DIRECTION('center_axis',(0.,-1.,0.));
#22412=DIRECTION('ref_axis',(0.971857119210143,0.,-0.235571092964656));
#22413=DIRECTION('',(0.,1.,0.));
#22414=DIRECTION('center_axis',(0.,-1.,0.));
#22415=DIRECTION('ref_axis',(0.528694902398929,0.,-0.848811934516349));
#22416=DIRECTION('center_axis',(0.,-1.,0.));
#22417=DIRECTION('ref_axis',(0.528694902399131,0.,-0.848811934516223));
#22418=DIRECTION('',(0.,1.,0.));
#22419=DIRECTION('center_axis',(0.,1.,0.));
#22420=DIRECTION('ref_axis',(0.528694902399131,0.,-0.848811934516223));
#22421=DIRECTION('center_axis',(0.,-1.,0.));
#22422=DIRECTION('ref_axis',(-0.281918008728675,0.,-0.959438500558769));
#22423=DIRECTION('center_axis',(0.,1.,0.));
#22424=DIRECTION('ref_axis',(-0.281918008754676,0.,-0.959438500551129));
#22425=DIRECTION('',(0.,-1.,0.));
#22426=DIRECTION('center_axis',(0.,-1.,0.));
#22427=DIRECTION('ref_axis',(-0.281918008754676,0.,-0.959438500551129));
#22428=DIRECTION('center_axis',(-0.882269183586981,0.,-0.470745247127108));
#22429=DIRECTION('ref_axis',(-0.470745247127108,0.,0.882269183586981));
#22430=DIRECTION('',(0.470745247127471,0.,-0.882269183586787));
#22431=DIRECTION('',(0.,1.,0.));
#22432=DIRECTION('',(-0.470745247127471,0.,0.882269183586787));
#22433=DIRECTION('center_axis',(0.848811934516349,0.,0.528694902398929));
#22434=DIRECTION('ref_axis',(0.,-1.,0.));
#22435=DIRECTION('',(0.528694902399201,0.,-0.84881193451618));
#22436=DIRECTION('',(0.,-1.,0.));
#22437=DIRECTION('',(-0.528694902399201,0.,0.84881193451618));
#22438=DIRECTION('center_axis',(0.772541698292714,0.,0.634964033941301));
#22439=DIRECTION('ref_axis',(0.,-1.,0.));
#22440=DIRECTION('',(0.634964033941407,0.,-0.772541698292626));
#22441=DIRECTION('',(0.,-1.,0.));
#22442=DIRECTION('',(-0.634964033941407,0.,0.772541698292626));
#22443=DIRECTION('center_axis',(0.581877193327018,0.,0.813276663802591));
#22444=DIRECTION('ref_axis',(0.,-1.,0.));
#22445=DIRECTION('',(0.813276663802457,0.,-0.581877193327205));
#22446=DIRECTION('',(0.,-1.,0.));
#22447=DIRECTION('',(-0.813276663802457,0.,0.581877193327205));
#22448=DIRECTION('center_axis',(0.470745247127107,0.,0.882269183586982));
#22449=DIRECTION('ref_axis',(0.,-1.,0.));
#22450=DIRECTION('',(0.882269183586788,0.,-0.470745247127471));
#22451=DIRECTION('',(0.,-1.,0.));
#22452=DIRECTION('',(-0.882269183586788,0.,0.470745247127471));
#22453=DIRECTION('center_axis',(0.,1.,0.));
#22454=DIRECTION('ref_axis',(-0.902585284349861,0.,0.430511096808295));
#22455=DIRECTION('center_axis',(0.,-1.,0.));
#22456=DIRECTION('ref_axis',(-0.902585284349705,0.,0.430511096808622));
#22457=DIRECTION('',(0.,1.,0.));
#22458=DIRECTION('center_axis',(0.,1.,0.));
#22459=DIRECTION('ref_axis',(-0.902585284349705,0.,0.430511096808622));
#22460=DIRECTION('center_axis',(0.,1.,0.));
#22461=DIRECTION('ref_axis',(-0.902585284349861,0.,0.430511096808295));
#22462=DIRECTION('center_axis',(0.,1.,0.));
#22463=DIRECTION('ref_axis',(-0.902585284349705,0.,0.430511096808622));
#22464=DIRECTION('center_axis',(0.,-1.,0.));
#22465=DIRECTION('ref_axis',(-0.902585284349705,0.,0.430511096808622));
#22466=DIRECTION('center_axis',(0.,1.,0.));
#22467=DIRECTION('ref_axis',(1.,0.,0.));
#22468=DIRECTION('',(0.430511096808718,0.,-0.902585284349659));
#22469=DIRECTION('center_axis',(0.,-1.,0.));
#22470=DIRECTION('ref_axis',(0.902585284349714,0.,-0.430511096808602));
#22471=DIRECTION('',(-0.902585284349657,0.,0.430511096808722));
#22472=DIRECTION('center_axis',(0.,1.,0.));
#22473=DIRECTION('ref_axis',(-0.902585284349705,0.,0.430511096808622));
#22474=DIRECTION('center_axis',(0.,1.,0.));
#22475=DIRECTION('ref_axis',(-0.902585284349705,0.,0.430511096808622));
#22476=DIRECTION('center_axis',(0.,1.,0.));
#22477=DIRECTION('ref_axis',(-0.902585284349705,0.,0.430511096808622));
#22478=DIRECTION('',(0.730368754817616,0.,-0.683053059422301));
#22479=DIRECTION('center_axis',(0.,1.,0.));
#22480=DIRECTION('ref_axis',(-0.902585284349705,0.,0.430511096808622));
#22481=DIRECTION('center_axis',(0.,1.,0.));
#22482=DIRECTION('ref_axis',(-0.902585284349861,0.,0.430511096808295));
#22483=DIRECTION('center_axis',(0.,-1.,0.));
#22484=DIRECTION('ref_axis',(-0.902585284349705,0.,0.430511096808622));
#22485=DIRECTION('',(0.,-1.,0.));
#22486=DIRECTION('center_axis',(0.,1.,0.));
#22487=DIRECTION('ref_axis',(-0.902585284349861,0.,0.430511096808295));
#22488=DIRECTION('',(0.,1.,0.));
#22489=DIRECTION('center_axis',(0.,-1.,0.));
#22490=DIRECTION('ref_axis',(-0.902585284349705,0.,0.430511096808622));
#22491=DIRECTION('center_axis',(0.683053059422266,0.,0.730368754817649));
#22492=DIRECTION('ref_axis',(0.,-1.,0.));
#22493=DIRECTION('',(-0.730368754817616,0.,0.683053059422301));
#22494=DIRECTION('center_axis',(0.,1.,0.));
#22495=DIRECTION('ref_axis',(-0.902585284349861,0.,0.430511096808295));
#22496=DIRECTION('center_axis',(0.,-1.,0.));
#22497=DIRECTION('ref_axis',(-0.902585284349705,0.,0.430511096808622));
#22498=DIRECTION('center_axis',(0.,1.,0.));
#22499=DIRECTION('ref_axis',(0.902585284349861,0.,-0.430511096808295));
#22500=DIRECTION('',(0.,-1.,0.));
#22501=DIRECTION('center_axis',(0.,1.,0.));
#22502=DIRECTION('ref_axis',(0.902585284349714,0.,-0.430511096808602));
#22503=DIRECTION('',(0.,1.,0.));
#22504=DIRECTION('center_axis',(0.430511096808296,0.,0.90258528434986));
#22505=DIRECTION('ref_axis',(0.,-1.,0.));
#22506=DIRECTION('',(0.902585284349657,0.,-0.430511096808722));
#22507=DIRECTION('center_axis',(0.,1.,0.));
#22508=DIRECTION('ref_axis',(-0.902585284349861,0.,0.430511096808295));
#22509=DIRECTION('center_axis',(0.,-1.,0.));
#22510=DIRECTION('ref_axis',(-0.902585284349705,0.,0.430511096808622));
#22511=DIRECTION('center_axis',(-0.902585284349862,0.,-0.430511096808292));
#22512=DIRECTION('ref_axis',(-0.430511096808292,0.,0.902585284349862));
#22513=DIRECTION('',(-0.430511096808718,0.,0.902585284349659));
#22514=DIRECTION('center_axis',(0.,1.,0.));
#22515=DIRECTION('ref_axis',(1.,0.,0.));
#22516=DIRECTION('axis',(0.,0.,1.));
#22517=DIRECTION('refdir',(1.,0.,0.));
#22518=DIRECTION('center_axis',(-2.07638679158937E-16,1.,-9.61039042249231E-32));
#22519=DIRECTION('ref_axis',(0.999984788371283,2.07635520636442E-16,-0.00551570721125971));
#22520=DIRECTION('center_axis',(2.07638679158937E-16,-1.,9.61039042249231E-32));
#22521=DIRECTION('ref_axis',(-0.999984788371283,-2.07635520636442E-16,0.00551570721125971));
#22522=DIRECTION('center_axis',(-2.07638679158937E-16,1.,-9.61039042249231E-32));
#22523=DIRECTION('ref_axis',(0.999984788371283,2.07635520636442E-16,-0.00551570721125971));
#22524=DIRECTION('center_axis',(-2.07638679158937E-16,1.,-9.61039042249231E-32));
#22525=DIRECTION('ref_axis',(0.999984788371283,2.07635520636442E-16,-0.00551570721125971));
#22526=DIRECTION('',(-2.07638679158937E-16,1.,-9.61039042249231E-32));
#22527=DIRECTION('center_axis',(2.07638679158937E-16,-1.,9.61039042249231E-32));
#22528=DIRECTION('ref_axis',(0.999984788371283,2.07635520636442E-16,-0.00551570721125971));
#22529=DIRECTION('center_axis',(-2.07638679158937E-16,1.,-9.61039042249231E-32));
#22530=DIRECTION('ref_axis',(-0.999984788371283,-2.07635520636442E-16,0.00551570721125971));
#22531=DIRECTION('center_axis',(-2.07638679158937E-16,1.,-9.61039042249231E-32));
#22532=DIRECTION('ref_axis',(-0.999984788371283,-2.07635520636442E-16,0.00551570721125971));
#22533=DIRECTION('',(2.07638679158937E-16,-1.,9.61039042249231E-32));
#22534=DIRECTION('center_axis',(-2.07638679158937E-16,1.,-9.61039042249231E-32));
#22535=DIRECTION('ref_axis',(0.999984788371283,2.07635520636442E-16,-0.00551570721125971));
#22536=DIRECTION('axis',(0.,0.,1.));
#22537=DIRECTION('refdir',(1.,0.,0.));
#22538=DIRECTION('center_axis',(0.,-1.,0.));
#22539=DIRECTION('ref_axis',(1.,0.,0.));
#22540=DIRECTION('center_axis',(0.3582068848149,-0.554700196225404,0.75099635150825));
#22541=DIRECTION('ref_axis',(0.238804589876937,0.832050294337727,0.500664234338952));
#22542=DIRECTION('center_axis',(0.,1.,0.));
#22543=DIRECTION('ref_axis',(1.,0.,0.));
#22544=DIRECTION('center_axis',(-0.75099635150825,-0.554700196225404,-0.3582068848149));
#22545=DIRECTION('ref_axis',(0.500664234338953,-0.832050294337727,0.238804589876937));
#22546=DIRECTION('',(0.,1.,0.));
#22547=DIRECTION('center_axis',(-0.75099635150825,0.554700196225404,-0.3582068848149));
#22548=DIRECTION('ref_axis',(0.500664234338953,0.832050294337727,0.238804589876937));
#22549=DIRECTION('center_axis',(0.,1.,0.));
#22550=DIRECTION('ref_axis',(1.,0.,0.));
#22551=DIRECTION('center_axis',(0.3582068848149,0.554700196225404,0.75099635150825));
#22552=DIRECTION('ref_axis',(0.238804589876937,-0.832050294337727,0.500664234338952));
#22553=DIRECTION('',(0.,-1.,0.));
#22554=DIRECTION('',(0.,1.,0.));
#22555=DIRECTION('',(0.,-1.,0.));
#22556=DIRECTION('center_axis',(-0.430511096808295,0.,-0.902585284349861));
#22557=DIRECTION('ref_axis',(-0.902585284349861,0.,0.430511096808295));
#22558=DIRECTION('',(-0.902585284349657,0.,0.430511096808721));
#22559=DIRECTION('',(0.902585284349657,0.,-0.430511096808721));
#22560=DIRECTION('',(0.,1.,0.));
#22561=DIRECTION('center_axis',(0.35820688481505,0.554700196225229,0.750996351508308));
#22562=DIRECTION('ref_axis',(0.84006490861712,-0.542485897798375,-2.44189949696171E-17));
#22563=DIRECTION('',(-0.902585284349657,0.,0.430511096808721));
#22564=DIRECTION('center_axis',(-0.358206884814892,-0.554700196225413,-0.750996351508247));
#22565=DIRECTION('ref_axis',(-0.238804589876949,0.832050294337721,-0.500664234338957));
#22566=DIRECTION('center_axis',(0.,1.,0.));
#22567=DIRECTION('ref_axis',(1.,0.,0.));
#22568=DIRECTION('',(0.430511096808721,0.,-0.902585284349657));
#22569=DIRECTION('center_axis',(0.,-1.,0.));
#22570=DIRECTION('ref_axis',(-1.,0.,0.));
#22571=DIRECTION('center_axis',(-0.750996351508308,0.554700196225229,-0.35820688481505));
#22572=DIRECTION('ref_axis',(-0.430511096808295,9.35899339744592E-17,0.902585284349861));
#22573=DIRECTION('center_axis',(0.750996351508247,-0.554700196225414,0.358206884814892));
#22574=DIRECTION('ref_axis',(-0.500664234338957,-0.83205029433772,-0.23880458987695));
#22575=DIRECTION('',(-0.430511096808721,0.,0.902585284349657));
#22576=DIRECTION('center_axis',(0.902585284349861,0.,0.430511096808295));
#22577=DIRECTION('ref_axis',(0.,-1.,0.));
#22578=DIRECTION('',(0.430511096808721,0.,-0.902585284349657));
#22579=DIRECTION('',(0.,-1.,0.));
#22580=DIRECTION('center_axis',(-0.750996351508308,-0.554700196225229,-0.35820688481505));
#22581=DIRECTION('ref_axis',(-0.594125001994256,0.804372725796521,-4.34111046316595E-17));
#22582=DIRECTION('',(-0.430511096808721,0.,0.902585284349657));
#22583=DIRECTION('center_axis',(0.750996351508247,0.554700196225413,0.358206884814892));
#22584=DIRECTION('ref_axis',(-0.500664234338957,0.832050294337721,-0.238804589876949));
#22585=DIRECTION('center_axis',(0.,-1.,0.));
#22586=DIRECTION('ref_axis',(-1.,0.,0.));
#22587=DIRECTION('center_axis',(-0.358206884814892,0.554700196225413,-0.750996351508247));
#22588=DIRECTION('ref_axis',(-0.238804589876949,-0.832050294337721,-0.500664234338957));
#22589=DIRECTION('center_axis',(0.,-1.,0.));
#22590=DIRECTION('ref_axis',(-1.,0.,0.));
#22591=DIRECTION('center_axis',(0.,-1.,0.));
#22592=DIRECTION('ref_axis',(0.,0.,-1.));
#22593=DIRECTION('',(0.902585284349657,0.,-0.430511096808721));
#22594=DIRECTION('center_axis',(0.35820688481505,-0.554700196225229,0.750996351508308));
#22595=DIRECTION('ref_axis',(-0.84006490861712,-0.542485897798375,2.44189949696171E-17));
#22596=DIRECTION('center_axis',(-0.707106781186548,1.63268091856641E-16,
-0.707106781186548));
#22597=DIRECTION('ref_axis',(-0.707106781186548,1.6035606412684E-33,0.707106781186548));
#22598=DIRECTION('',(-0.707106781186548,0.,0.707106781186548));
#22599=DIRECTION('',(-1.0001154479739E-12,-1.,-1.0001154479739E-12));
#22600=DIRECTION('',(-0.707106781186548,0.,0.707106781186548));
#22601=DIRECTION('center_axis',(-0.707106781186548,0.,0.707106781186548));
#22602=DIRECTION('ref_axis',(0.707106781186547,0.,0.707106781186547));
#22603=DIRECTION('',(-0.707106781186548,0.,0.707106781186548));
#22604=DIRECTION('center_axis',(-0.707106781186548,0.,0.707106781186548));
#22605=DIRECTION('ref_axis',(0.707106781186547,0.,0.707106781186547));
#22606=DIRECTION('center_axis',(-0.707106781186548,0.,0.707106781186548));
#22607=DIRECTION('ref_axis',(-0.707106781186547,0.,-0.707106781186547));
#22608=DIRECTION('center_axis',(-0.707106781186548,0.,0.707106781186548));
#22609=DIRECTION('ref_axis',(-0.707106781186547,0.,-0.707106781186547));
#22610=DIRECTION('',(-0.707106781186548,0.,0.707106781186548));
#22611=DIRECTION('center_axis',(0.707106781186548,8.16340459283203E-17,
0.707106781186548));
#22612=DIRECTION('ref_axis',(-1.81589014284111E-31,-1.,1.15447974903219E-16));
#22613=DIRECTION('',(-1.00005772398645E-12,1.,-1.00005772398645E-12));
#22614=DIRECTION('center_axis',(0.,-1.,0.));
#22615=DIRECTION('ref_axis',(0.707106781186548,0.,-0.707106781186548));
#22616=DIRECTION('center_axis',(0.784325130117969,-0.554700196225389,0.277744095478098));
#22617=DIRECTION('ref_axis',(0.522883420078948,0.832050294337737,0.185162730318571));
#22618=DIRECTION('center_axis',(0.,1.,0.));
#22619=DIRECTION('ref_axis',(0.707106781186547,0.,-0.707106781186547));
#22620=DIRECTION('center_axis',(-0.784325130117969,-0.554700196225389,0.277744095478098));
#22621=DIRECTION('ref_axis',(0.522883420078948,-0.832050294337737,-0.185162730318571));
#22622=DIRECTION('',(0.,1.,0.));
#22623=DIRECTION('center_axis',(-0.784325130117969,0.554700196225389,0.277744095478098));
#22624=DIRECTION('ref_axis',(0.522883420078948,0.832050294337737,-0.185162730318571));
#22625=DIRECTION('center_axis',(0.,1.,0.));
#22626=DIRECTION('ref_axis',(0.707106781186547,0.,-0.707106781186547));
#22627=DIRECTION('center_axis',(0.784325130117969,0.554700196225389,0.277744095478098));
#22628=DIRECTION('ref_axis',(0.522883420078948,-0.832050294337737,0.185162730318571));
#22629=DIRECTION('',(0.,-1.,0.));
#22630=DIRECTION('',(0.,1.,0.));
#22631=DIRECTION('',(0.,-1.,0.));
#22632=DIRECTION('center_axis',(-0.942641491092178,0.,-0.333806859233771));
#22633=DIRECTION('ref_axis',(-0.333806859233771,0.,0.942641491092178));
#22634=DIRECTION('',(-0.333806859234345,0.,0.942641491091975));
#22635=DIRECTION('',(0.333806859234345,0.,-0.942641491091975));
#22636=DIRECTION('',(0.,1.,0.));
#22637=DIRECTION('center_axis',(0.784325130118311,0.554700196225229,0.27774409547745));
#22638=DIRECTION('ref_axis',(1.41728662356081E-16,0.447721620230319,-0.894172998238226));
#22639=DIRECTION('',(-0.333806859234345,0.,0.942641491091975));
#22640=DIRECTION('center_axis',(-0.78432513011795,-0.554700196225397,-0.277744095478133));
#22641=DIRECTION('ref_axis',(-0.522883420078951,0.832050294337732,-0.185162730318585));
#22642=DIRECTION('center_axis',(0.,1.,0.));
#22643=DIRECTION('ref_axis',(1.,0.,0.));
#22644=DIRECTION('',(-0.333806859234345,0.,-0.942641491091975));
#22645=DIRECTION('center_axis',(0.,-1.,0.));
#22646=DIRECTION('ref_axis',(-0.707106781186548,0.,0.707106781186548));
#22647=DIRECTION('center_axis',(-0.784325130118311,0.554700196225229,0.27774409547745));
#22648=DIRECTION('ref_axis',(0.333806859233771,9.47580827855939E-17,0.942641491092179));
#22649=DIRECTION('center_axis',(0.78432513011795,-0.554700196225398,-0.277744095478132));
#22650=DIRECTION('ref_axis',(-0.522883420078952,-0.832050294337731,0.185162730318585));
#22651=DIRECTION('',(0.333806859234345,0.,0.942641491091975));
#22652=DIRECTION('center_axis',(0.942641491092178,0.,-0.333806859233771));
#22653=DIRECTION('ref_axis',(0.,-1.,0.));
#22654=DIRECTION('',(-0.333806859234345,0.,-0.942641491091975));
#22655=DIRECTION('',(0.,-1.,0.));
#22656=DIRECTION('center_axis',(-0.784325130118311,-0.554700196225229,0.27774409547745));
#22657=DIRECTION('ref_axis',(-0.577418677468947,0.816448204670702,-1.57337619069903E-16));
#22658=DIRECTION('',(0.333806859234345,0.,0.942641491091975));
#22659=DIRECTION('center_axis',(0.78432513011795,0.554700196225397,-0.277744095478133));
#22660=DIRECTION('ref_axis',(-0.522883420078951,0.832050294337732,0.185162730318585));
#22661=DIRECTION('center_axis',(0.,-1.,0.));
#22662=DIRECTION('ref_axis',(-0.707106781186548,0.,0.707106781186548));
#22663=DIRECTION('center_axis',(-0.78432513011795,0.554700196225397,-0.277744095478133));
#22664=DIRECTION('ref_axis',(-0.522883420078951,-0.832050294337732,-0.185162730318585));
#22665=DIRECTION('center_axis',(0.,-1.,0.));
#22666=DIRECTION('ref_axis',(-0.707106781186548,0.,0.707106781186548));
#22667=DIRECTION('center_axis',(0.,-1.,0.));
#22668=DIRECTION('ref_axis',(0.,0.,-1.));
#22669=DIRECTION('',(0.333806859234345,0.,-0.942641491091975));
#22670=DIRECTION('center_axis',(0.784325130118311,-0.554700196225229,0.27774409547745));
#22671=DIRECTION('ref_axis',(1.41728662356081E-16,-0.447721620230319,-0.894172998238226));
#22672=DIRECTION('center_axis',(-1.,1.63268091856641E-16,0.));
#22673=DIRECTION('ref_axis',(0.,0.,1.));
#22674=DIRECTION('',(0.,0.,1.));
#22675=DIRECTION('',(-1.00016326809086E-12,-1.,0.));
#22676=DIRECTION('',(0.,0.,1.));
#22677=DIRECTION('center_axis',(0.,0.,1.));
#22678=DIRECTION('ref_axis',(1.,0.,0.));
#22679=DIRECTION('',(0.,0.,1.));
#22680=DIRECTION('center_axis',(0.,0.,1.));
#22681=DIRECTION('ref_axis',(1.,0.,0.));
#22682=DIRECTION('center_axis',(0.,0.,1.));
#22683=DIRECTION('ref_axis',(-1.,0.,0.));
#22684=DIRECTION('center_axis',(0.,0.,1.));
#22685=DIRECTION('ref_axis',(-1.,0.,0.));
#22686=DIRECTION('',(0.,0.,1.));
#22687=DIRECTION('center_axis',(1.,5.4401887036275E-49,6.66411745462711E-33));
#22688=DIRECTION('ref_axis',(4.75910974851396E-64,1.,-8.16340459283203E-17));
#22689=DIRECTION('',(-1.00008163404493E-12,1.,0.));
#22690=DIRECTION('center_axis',(0.,-1.,0.));
#22691=DIRECTION('ref_axis',(0.,0.,-1.));
#22692=DIRECTION('center_axis',(0.75099635150825,-0.554700196225404,-0.3582068848149));
#22693=DIRECTION('ref_axis',(0.500664234338953,0.832050294337727,-0.238804589876937));
#22694=DIRECTION('center_axis',(0.,1.,0.));
#22695=DIRECTION('ref_axis',(0.,0.,-1.));
#22696=DIRECTION('center_axis',(-0.3582068848149,-0.554700196225404,0.75099635150825));
#22697=DIRECTION('ref_axis',(0.238804589876937,-0.832050294337727,-0.500664234338952));
#22698=DIRECTION('',(0.,1.,0.));
#22699=DIRECTION('center_axis',(-0.3582068848149,0.554700196225404,0.75099635150825));
#22700=DIRECTION('ref_axis',(0.238804589876937,0.832050294337727,-0.500664234338953));
#22701=DIRECTION('center_axis',(0.,1.,0.));
#22702=DIRECTION('ref_axis',(0.,0.,-1.));
#22703=DIRECTION('center_axis',(0.75099635150825,0.554700196225404,-0.3582068848149));
#22704=DIRECTION('ref_axis',(0.500664234338953,-0.832050294337727,-0.238804589876937));
#22705=DIRECTION('',(0.,-1.,0.));
#22706=DIRECTION('',(0.,1.,0.));
#22707=DIRECTION('',(0.,-1.,0.));
#22708=DIRECTION('center_axis',(-0.902585284349861,0.,0.430511096808295));
#22709=DIRECTION('ref_axis',(0.,1.,0.));
#22710=DIRECTION('',(0.430511096808721,0.,0.902585284349657));
#22711=DIRECTION('',(-0.430511096808721,0.,-0.902585284349657));
#22712=DIRECTION('',(0.,1.,0.));
#22713=DIRECTION('center_axis',(0.750996351508308,0.554700196225229,-0.35820688481505));
#22714=DIRECTION('ref_axis',(-2.67556946657892E-17,-0.542485897798375,-0.84006490861712));
#22715=DIRECTION('',(0.430511096808721,0.,0.902585284349657));
#22716=DIRECTION('center_axis',(-0.750996351508247,-0.554700196225413,0.358206884814892));
#22717=DIRECTION('ref_axis',(-0.500664234338957,0.832050294337721,0.238804589876949));
#22718=DIRECTION('center_axis',(0.,1.,0.));
#22719=DIRECTION('ref_axis',(1.,0.,0.));
#22720=DIRECTION('',(-0.902585284349657,0.,-0.430511096808721));
#22721=DIRECTION('center_axis',(0.,-1.,0.));
#22722=DIRECTION('ref_axis',(0.,0.,1.));
#22723=DIRECTION('center_axis',(-0.35820688481505,0.554700196225229,0.750996351508308));
#22724=DIRECTION('ref_axis',(0.84006490861712,0.542485897798375,2.44189949696171E-17));
#22725=DIRECTION('center_axis',(0.358206884814892,-0.554700196225414,-0.750996351508247));
#22726=DIRECTION('ref_axis',(-0.23880458987695,-0.83205029433772,0.500664234338957));
#22727=DIRECTION('',(0.902585284349657,0.,0.430511096808721));
#22728=DIRECTION('center_axis',(0.430511096808295,0.,-0.902585284349861));
#22729=DIRECTION('ref_axis',(0.,-1.,0.));
#22730=DIRECTION('',(-0.902585284349657,0.,-0.430511096808721));
#22731=DIRECTION('',(0.,-1.,0.));
#22732=DIRECTION('center_axis',(-0.35820688481505,-0.554700196225229,0.750996351508308));
#22733=DIRECTION('ref_axis',(-0.84006490861712,0.542485897798375,-2.44189949696171E-17));
#22734=DIRECTION('',(0.902585284349657,0.,0.430511096808721));
#22735=DIRECTION('center_axis',(0.358206884814892,0.554700196225413,-0.750996351508247));
#22736=DIRECTION('ref_axis',(-0.238804589876949,0.832050294337721,0.500664234338957));
#22737=DIRECTION('center_axis',(0.,-1.,0.));
#22738=DIRECTION('ref_axis',(0.,0.,1.));
#22739=DIRECTION('center_axis',(-0.750996351508247,0.554700196225413,0.358206884814892));
#22740=DIRECTION('ref_axis',(-0.500664234338957,-0.832050294337721,0.238804589876949));
#22741=DIRECTION('center_axis',(0.,-1.,0.));
#22742=DIRECTION('ref_axis',(0.,0.,1.));
#22743=DIRECTION('center_axis',(0.,-1.,0.));
#22744=DIRECTION('ref_axis',(0.,0.,-1.));
#22745=DIRECTION('',(-0.430511096808721,0.,-0.902585284349657));
#22746=DIRECTION('center_axis',(0.750996351508308,-0.554700196225229,-0.35820688481505));
#22747=DIRECTION('ref_axis',(-2.67556946657892E-17,0.542485897798375,-0.84006490861712));
#22748=DIRECTION('center_axis',(-0.707106781186548,1.63268091856641E-16,
0.707106781186548));
#22749=DIRECTION('ref_axis',(2.30895949806438E-16,1.,9.37581606751804E-32));
#22750=DIRECTION('',(0.707106781186548,0.,0.707106781186548));
#22751=DIRECTION('',(-1.0001154479739E-12,-1.,1.0001154479739E-12));
#22752=DIRECTION('',(0.707106781186548,0.,0.707106781186548));
#22753=DIRECTION('center_axis',(0.707106781186548,0.,0.707106781186548));
#22754=DIRECTION('ref_axis',(0.707106781186547,0.,-0.707106781186547));
#22755=DIRECTION('',(0.707106781186548,0.,0.707106781186548));
#22756=DIRECTION('center_axis',(0.707106781186548,0.,0.707106781186548));
#22757=DIRECTION('ref_axis',(0.707106781186547,0.,-0.707106781186547));
#22758=DIRECTION('center_axis',(0.707106781186548,0.,0.707106781186548));
#22759=DIRECTION('ref_axis',(-0.707106781186547,0.,0.707106781186547));
#22760=DIRECTION('center_axis',(0.707106781186548,0.,0.707106781186548));
#22761=DIRECTION('ref_axis',(-0.707106781186547,0.,0.707106781186547));
#22762=DIRECTION('',(0.707106781186548,0.,0.707106781186548));
#22763=DIRECTION('center_axis',(0.707106781186548,8.16340459283203E-17,
-0.707106781186548));
#22764=DIRECTION('ref_axis',(-1.81589014284111E-31,-1.,-1.15447974903219E-16));
#22765=DIRECTION('',(-1.00005772398645E-12,1.,1.00005772398645E-12));
#22766=DIRECTION('center_axis',(0.,-1.,0.));
#22767=DIRECTION('ref_axis',(-0.707106781186547,0.,-0.707106781186548));
#22768=DIRECTION('center_axis',(0.277744095478098,-0.554700196225389,-0.784325130117969));
#22769=DIRECTION('ref_axis',(0.185162730318571,0.832050294337737,-0.522883420078948));
#22770=DIRECTION('center_axis',(0.,1.,0.));
#22771=DIRECTION('ref_axis',(-0.707106781186547,0.,-0.707106781186548));
#22772=DIRECTION('center_axis',(0.277744095478098,-0.554700196225389,0.784325130117969));
#22773=DIRECTION('ref_axis',(-0.185162730318571,-0.832050294337737,-0.522883420078948));
#22774=DIRECTION('',(0.,1.,0.));
#22775=DIRECTION('center_axis',(0.277744095478098,0.554700196225389,0.784325130117969));
#22776=DIRECTION('ref_axis',(-0.185162730318571,0.832050294337737,-0.522883420078948));
#22777=DIRECTION('center_axis',(0.,1.,0.));
#22778=DIRECTION('ref_axis',(-0.707106781186547,0.,-0.707106781186548));
#22779=DIRECTION('center_axis',(0.277744095478098,0.554700196225389,-0.784325130117969));
#22780=DIRECTION('ref_axis',(0.185162730318571,-0.832050294337737,-0.522883420078948));
#22781=DIRECTION('',(0.,-1.,0.));
#22782=DIRECTION('',(0.,1.,0.));
#22783=DIRECTION('',(0.,-1.,0.));
#22784=DIRECTION('center_axis',(-0.333806859233771,0.,0.942641491092178));
#22785=DIRECTION('ref_axis',(0.,1.,0.));
#22786=DIRECTION('',(0.942641491091975,0.,0.333806859234345));
#22787=DIRECTION('',(-0.942641491091975,0.,-0.333806859234345));
#22788=DIRECTION('',(0.,1.,0.));
#22789=DIRECTION('center_axis',(0.27774409547745,0.554700196225229,-0.784325130118311));
#22790=DIRECTION('ref_axis',(-0.942641491092179,-8.22449654774124E-17,-0.333806859233771));
#22791=DIRECTION('',(0.942641491091975,0.,0.333806859234345));
#22792=DIRECTION('center_axis',(-0.277744095478133,-0.554700196225397,0.78432513011795));
#22793=DIRECTION('ref_axis',(-0.185162730318585,0.832050294337732,0.522883420078951));
#22794=DIRECTION('center_axis',(0.,1.,0.));
#22795=DIRECTION('ref_axis',(1.,0.,0.));
#22796=DIRECTION('',(-0.942641491091975,0.,0.333806859234345));
#22797=DIRECTION('center_axis',(0.,-1.,0.));
#22798=DIRECTION('ref_axis',(0.707106781186547,0.,0.707106781186548));
#22799=DIRECTION('center_axis',(0.27774409547745,0.554700196225229,0.784325130118311));
#22800=DIRECTION('ref_axis',(0.894172998238226,-0.447721620230319,-1.29766088156978E-16));
#22801=DIRECTION('center_axis',(-0.277744095478132,-0.554700196225398,-0.78432513011795));
#22802=DIRECTION('ref_axis',(0.185162730318585,-0.832050294337731,0.522883420078952));
#22803=DIRECTION('',(0.942641491091975,0.,-0.333806859234345));
#22804=DIRECTION('center_axis',(-0.333806859233771,0.,-0.942641491092178));
#22805=DIRECTION('ref_axis',(-0.942641491092178,0.,0.333806859233771));
#22806=DIRECTION('',(-0.942641491091975,0.,0.333806859234345));
#22807=DIRECTION('',(0.,-1.,0.));
#22808=DIRECTION('center_axis',(0.27774409547745,-0.554700196225229,0.784325130118311));
#22809=DIRECTION('ref_axis',(-0.894172998238226,-0.447721620230319,1.29766088156978E-16));
#22810=DIRECTION('',(0.942641491091975,0.,-0.333806859234345));
#22811=DIRECTION('center_axis',(-0.277744095478133,0.554700196225397,-0.78432513011795));
#22812=DIRECTION('ref_axis',(0.185162730318585,0.832050294337732,0.522883420078951));
#22813=DIRECTION('center_axis',(0.,-1.,0.));
#22814=DIRECTION('ref_axis',(0.707106781186547,0.,0.707106781186548));
#22815=DIRECTION('center_axis',(-0.277744095478133,0.554700196225397,0.78432513011795));
#22816=DIRECTION('ref_axis',(-0.185162730318585,-0.832050294337732,0.522883420078951));
#22817=DIRECTION('center_axis',(0.,-1.,0.));
#22818=DIRECTION('ref_axis',(0.707106781186547,0.,0.707106781186548));
#22819=DIRECTION('center_axis',(0.,-1.,0.));
#22820=DIRECTION('ref_axis',(0.,0.,-1.));
#22821=DIRECTION('',(-0.942641491091975,0.,-0.333806859234345));
#22822=DIRECTION('center_axis',(0.27774409547745,-0.554700196225229,-0.784325130118311));
#22823=DIRECTION('ref_axis',(1.53589745588664E-16,-0.816448204670702,0.577418677468947));
#22824=DIRECTION('center_axis',(-1.81263994765859E-32,1.63268091856641E-16,
1.));
#22825=DIRECTION('ref_axis',(1.,1.11022302462516E-16,5.86020957047602E-47));
#22826=DIRECTION('',(1.,0.,1.00011102230146E-12));
#22827=DIRECTION('',(-9.99999999999E-13,-1.,1.00016326809086E-12));
#22828=DIRECTION('',(1.,0.,1.00011102230146E-12));
#22829=DIRECTION('center_axis',(1.,0.,1.85037170770859E-16));
#22830=DIRECTION('ref_axis',(1.85037170770859E-16,0.,-1.));
#22831=DIRECTION('',(1.,0.,1.00011102230146E-12));
#22832=DIRECTION('center_axis',(1.,0.,6.66685170379299E-12));
#22833=DIRECTION('ref_axis',(6.66685170379299E-12,0.,-1.));
#22834=DIRECTION('center_axis',(1.,0.,9.25185853854296E-17));
#22835=DIRECTION('ref_axis',(-9.25185853854296E-17,0.,1.));
#22836=DIRECTION('center_axis',(1.,0.,6.66675918520761E-12));
#22837=DIRECTION('ref_axis',(-6.66675918520761E-12,0.,1.));
#22838=DIRECTION('',(1.,0.,1.00011102230146E-12));
#22839=DIRECTION('center_axis',(1.11022302462516E-16,8.16340459283203E-17,
-1.));
#22840=DIRECTION('ref_axis',(0.,-1.,-8.16340459283203E-17));
#22841=DIRECTION('',(-9.99999999999E-13,1.,1.00008163404493E-12));
#22842=DIRECTION('center_axis',(0.,-1.,0.));
#22843=DIRECTION('ref_axis',(-1.,0.,-1.51566283225277E-16));
#22844=DIRECTION('center_axis',(-0.3582068848149,-0.554700196225404,-0.75099635150825));
#22845=DIRECTION('ref_axis',(-0.238804589876937,0.832050294337727,-0.500664234338952));
#22846=DIRECTION('center_axis',(0.,1.,0.));
#22847=DIRECTION('ref_axis',(-1.,0.,-6.82745422938049E-13));
#22848=DIRECTION('center_axis',(0.75099635150825,-0.554700196225404,0.3582068848149));
#22849=DIRECTION('ref_axis',(-0.500664234338953,-0.832050294337727,-0.238804589876937));
#22850=DIRECTION('',(0.,1.,0.));
#22851=DIRECTION('center_axis',(0.75099635150825,0.554700196225404,0.3582068848149));
#22852=DIRECTION('ref_axis',(-0.500664234338953,0.832050294337727,-0.238804589876937));
#22853=DIRECTION('center_axis',(0.,1.,0.));
#22854=DIRECTION('ref_axis',(-1.,0.,-6.82745422938049E-13));
#22855=DIRECTION('center_axis',(-0.3582068848149,0.554700196225404,-0.75099635150825));
#22856=DIRECTION('ref_axis',(-0.238804589876937,-0.832050294337727,-0.500664234338952));
#22857=DIRECTION('',(0.,-1.,0.));
#22858=DIRECTION('',(0.,1.,0.));
#22859=DIRECTION('',(0.,-1.,0.));
#22860=DIRECTION('center_axis',(0.430511096808295,0.,0.902585284349861));
#22861=DIRECTION('ref_axis',(0.,-1.,0.));
#22862=DIRECTION('',(0.902585284349657,0.,-0.430511096808721));
#22863=DIRECTION('',(-0.902585284349657,0.,0.430511096808721));
#22864=DIRECTION('',(0.,1.,0.));
#22865=DIRECTION('center_axis',(-0.35820688481505,0.554700196225229,-0.750996351508308));
#22866=DIRECTION('ref_axis',(-0.902585284349861,-8.75902672829316E-17,0.430511096808295));
#22867=DIRECTION('',(0.902585284349657,0.,-0.430511096808721));
#22868=DIRECTION('center_axis',(0.358206884814892,-0.554700196225413,0.750996351508247));
#22869=DIRECTION('ref_axis',(0.238804589876949,0.832050294337721,0.500664234338957));
#22870=DIRECTION('center_axis',(0.,1.,0.));
#22871=DIRECTION('ref_axis',(1.,0.,0.));
#22872=DIRECTION('',(-0.430511096808721,0.,0.902585284349657));
#22873=DIRECTION('center_axis',(0.,-1.,0.));
#22874=DIRECTION('ref_axis',(1.,0.,7.19584204751227E-13));
#22875=DIRECTION('center_axis',(0.750996351508308,0.554700196225229,0.35820688481505));
#22876=DIRECTION('ref_axis',(2.67556946657892E-17,0.542485897798375,-0.84006490861712));
#22877=DIRECTION('center_axis',(-0.750996351508247,-0.554700196225414,-0.358206884814892));
#22878=DIRECTION('ref_axis',(0.500664234338957,-0.83205029433772,0.23880458987695));
#22879=DIRECTION('',(0.430511096808721,0.,-0.902585284349657));
#22880=DIRECTION('center_axis',(-0.902585284349861,0.,-0.430511096808295));
#22881=DIRECTION('ref_axis',(-0.430511096808295,0.,0.902585284349861));
#22882=DIRECTION('',(-0.430511096808721,0.,0.902585284349657));
#22883=DIRECTION('',(0.,-1.,0.));
#22884=DIRECTION('center_axis',(0.750996351508308,-0.554700196225229,0.35820688481505));
#22885=DIRECTION('ref_axis',(2.67556946657892E-17,-0.542485897798375,-0.84006490861712));
#22886=DIRECTION('',(0.430511096808721,0.,-0.902585284349657));
#22887=DIRECTION('center_axis',(-0.750996351508247,0.554700196225413,-0.358206884814892));
#22888=DIRECTION('ref_axis',(0.500664234338957,0.832050294337721,0.238804589876949));
#22889=DIRECTION('center_axis',(0.,-1.,0.));
#22890=DIRECTION('ref_axis',(1.,0.,1.59744320089951E-16));
#22891=DIRECTION('center_axis',(0.358206884814892,0.554700196225413,0.750996351508247));
#22892=DIRECTION('ref_axis',(0.238804589876949,-0.832050294337721,0.500664234338957));
#22893=DIRECTION('center_axis',(0.,-1.,0.));
#22894=DIRECTION('ref_axis',(1.,0.,7.19584204751227E-13));
#22895=DIRECTION('center_axis',(0.,-1.,0.));
#22896=DIRECTION('ref_axis',(0.,0.,-1.));
#22897=DIRECTION('',(-0.902585284349657,0.,0.430511096808721));
#22898=DIRECTION('center_axis',(-0.35820688481505,-0.554700196225229,-0.750996351508308));
#22899=DIRECTION('ref_axis',(4.41754862127715E-17,-0.804372725796521,0.594125001994256));
#22900=DIRECTION('center_axis',(0.707106781186547,1.63268091856641E-16,
0.707106781186548));
#22901=DIRECTION('ref_axis',(2.30895949806438E-16,-1.,7.31254524561613E-32));
#22902=DIRECTION('',(0.707106781186548,0.,-0.707106781186547));
#22903=DIRECTION('',(1.0001154479739E-12,-1.,1.0001154479739E-12));
#22904=DIRECTION('',(0.707106781186548,0.,-0.707106781186547));
#22905=DIRECTION('center_axis',(0.707106781186548,0.,-0.707106781186547));
#22906=DIRECTION('ref_axis',(-0.707106781186547,0.,-0.707106781186548));
#22907=DIRECTION('',(0.707106781186548,0.,-0.707106781186547));
#22908=DIRECTION('center_axis',(0.707106781186548,0.,-0.707106781186547));
#22909=DIRECTION('ref_axis',(-0.707106781186547,0.,-0.707106781186548));
#22910=DIRECTION('center_axis',(0.707106781186548,0.,-0.707106781186547));
#22911=DIRECTION('ref_axis',(0.707106781186547,0.,0.707106781186548));
#22912=DIRECTION('center_axis',(0.707106781186548,0.,-0.707106781186547));
#22913=DIRECTION('ref_axis',(0.707106781186547,0.,0.707106781186548));
#22914=DIRECTION('',(0.707106781186548,0.,-0.707106781186547));
#22915=DIRECTION('center_axis',(-0.707106781186547,8.16340459283203E-17,
-0.707106781186548));
#22916=DIRECTION('ref_axis',(-0.707106781186548,-2.19944674621426E-33,0.707106781186547));
#22917=DIRECTION('',(1.00005772398645E-12,1.,1.00005772398645E-12));
#22918=DIRECTION('center_axis',(0.,-1.,0.));
#22919=DIRECTION('ref_axis',(-0.707106781186548,0.,0.707106781186547));
#22920=DIRECTION('center_axis',(-0.784325130117969,-0.554700196225389,-0.277744095478098));
#22921=DIRECTION('ref_axis',(-0.522883420078948,0.832050294337737,-0.185162730318571));
#22922=DIRECTION('center_axis',(0.,1.,0.));
#22923=DIRECTION('ref_axis',(-0.707106781186548,0.,0.707106781186547));
#22924=DIRECTION('center_axis',(0.784325130117969,-0.554700196225389,-0.277744095478098));
#22925=DIRECTION('ref_axis',(-0.522883420078948,-0.832050294337737,0.185162730318571));
#22926=DIRECTION('',(0.,1.,0.));
#22927=DIRECTION('center_axis',(0.784325130117969,0.554700196225389,-0.277744095478098));
#22928=DIRECTION('ref_axis',(-0.522883420078948,0.832050294337737,0.185162730318571));
#22929=DIRECTION('center_axis',(0.,1.,0.));
#22930=DIRECTION('ref_axis',(-0.707106781186548,0.,0.707106781186547));
#22931=DIRECTION('center_axis',(-0.784325130117969,0.554700196225389,-0.277744095478098));
#22932=DIRECTION('ref_axis',(-0.522883420078948,-0.832050294337737,-0.185162730318571));
#22933=DIRECTION('',(0.,-1.,0.));
#22934=DIRECTION('',(0.,1.,0.));
#22935=DIRECTION('',(0.,-1.,0.));
#22936=DIRECTION('center_axis',(0.942641491092178,0.,0.333806859233771));
#22937=DIRECTION('ref_axis',(0.,-1.,0.));
#22938=DIRECTION('',(0.333806859234345,0.,-0.942641491091975));
#22939=DIRECTION('',(-0.333806859234345,0.,0.942641491091975));
#22940=DIRECTION('',(0.,1.,0.));
#22941=DIRECTION('center_axis',(-0.784325130118311,0.554700196225229,-0.27774409547745));
#22942=DIRECTION('ref_axis',(-0.333806859233771,-9.47580827855939E-17,0.942641491092179));
#22943=DIRECTION('',(0.333806859234345,0.,-0.942641491091975));
#22944=DIRECTION('center_axis',(0.78432513011795,-0.554700196225397,0.277744095478133));
#22945=DIRECTION('ref_axis',(0.522883420078951,0.832050294337732,0.185162730318585));
#22946=DIRECTION('center_axis',(0.,1.,0.));
#22947=DIRECTION('ref_axis',(1.,0.,0.));
#22948=DIRECTION('',(0.333806859234345,0.,0.942641491091975));
#22949=DIRECTION('center_axis',(0.,-1.,0.));
#22950=DIRECTION('ref_axis',(0.707106781186548,0.,-0.707106781186547));
#22951=DIRECTION('center_axis',(0.784325130118311,0.554700196225229,-0.27774409547745));
#22952=DIRECTION('ref_axis',(-1.41728662356081E-16,-0.447721620230319,-0.894172998238226));
#22953=DIRECTION('center_axis',(-0.78432513011795,-0.554700196225398,0.277744095478132));
#22954=DIRECTION('ref_axis',(0.522883420078952,-0.832050294337731,-0.185162730318585));
#22955=DIRECTION('',(-0.333806859234345,0.,-0.942641491091975));
#22956=DIRECTION('center_axis',(-0.942641491092178,0.,0.333806859233771));
#22957=DIRECTION('ref_axis',(0.,1.,0.));
#22958=DIRECTION('',(0.333806859234345,0.,0.942641491091975));
#22959=DIRECTION('',(0.,-1.,0.));
#22960=DIRECTION('center_axis',(0.784325130118311,-0.554700196225229,-0.27774409547745));
#22961=DIRECTION('ref_axis',(-1.41728662356081E-16,0.447721620230319,-0.894172998238226));
#22962=DIRECTION('',(-0.333806859234345,0.,-0.942641491091975));
#22963=DIRECTION('center_axis',(-0.78432513011795,0.554700196225397,0.277744095478133));
#22964=DIRECTION('ref_axis',(0.522883420078951,0.832050294337732,-0.185162730318585));
#22965=DIRECTION('center_axis',(0.,-1.,0.));
#22966=DIRECTION('ref_axis',(0.707106781186548,0.,-0.707106781186547));
#22967=DIRECTION('center_axis',(0.78432513011795,0.554700196225397,0.277744095478133));
#22968=DIRECTION('ref_axis',(0.522883420078951,-0.832050294337732,0.185162730318585));
#22969=DIRECTION('center_axis',(0.,-1.,0.));
#22970=DIRECTION('ref_axis',(0.707106781186548,0.,-0.707106781186547));
#22971=DIRECTION('center_axis',(0.,-1.,0.));
#22972=DIRECTION('ref_axis',(0.,0.,-1.));
#22973=DIRECTION('',(-0.333806859234345,0.,0.942641491091975));
#22974=DIRECTION('center_axis',(-0.784325130118311,-0.554700196225229,-0.27774409547745));
#22975=DIRECTION('ref_axis',(-0.577418677468947,0.816448204670702,1.57337619069903E-16));
#22976=DIRECTION('center_axis',(1.,1.81263994765859E-32,1.11022302462516E-16));
#22977=DIRECTION('ref_axis',(-5.86020957047602E-47,1.,-1.63268091856641E-16));
#22978=DIRECTION('',(1.00011102230146E-12,0.,-1.));
#22979=DIRECTION('',(1.00016326809086E-12,-1.,9.99999999999E-13));
#22980=DIRECTION('',(1.00011102230146E-12,0.,-1.));
#22981=DIRECTION('center_axis',(1.85037170770859E-16,0.,-1.));
#22982=DIRECTION('ref_axis',(-1.,0.,-1.85037170770859E-16));
#22983=DIRECTION('',(1.00011102230146E-12,0.,-1.));
#22984=DIRECTION('center_axis',(6.66685170379299E-12,0.,-1.));
#22985=DIRECTION('ref_axis',(-1.,0.,-6.66685170379299E-12));
#22986=DIRECTION('center_axis',(9.25185853854296E-17,0.,-1.));
#22987=DIRECTION('ref_axis',(1.,0.,9.25185853854296E-17));
#22988=DIRECTION('center_axis',(6.66675918520761E-12,0.,-1.));
#22989=DIRECTION('ref_axis',(1.,0.,6.66675918520761E-12));
#22990=DIRECTION('',(1.00011102230146E-12,0.,-1.));
#22991=DIRECTION('center_axis',(-1.,8.16340459283203E-17,-1.11022302462516E-16));
#22992=DIRECTION('ref_axis',(-1.11022302462516E-16,0.,1.));
#22993=DIRECTION('',(1.00008163404493E-12,1.,9.99999999999E-13));
#22994=DIRECTION('center_axis',(0.,-1.,0.));
#22995=DIRECTION('ref_axis',(-1.51566283225277E-16,0.,1.));
#22996=DIRECTION('center_axis',(-0.75099635150825,-0.554700196225404,0.3582068848149));
#22997=DIRECTION('ref_axis',(-0.500664234338953,0.832050294337727,0.238804589876937));
#22998=DIRECTION('center_axis',(0.,1.,0.));
#22999=DIRECTION('ref_axis',(-6.82745422938049E-13,0.,1.));
#23000=DIRECTION('center_axis',(0.3582068848149,-0.554700196225404,-0.75099635150825));
#23001=DIRECTION('ref_axis',(-0.238804589876937,-0.832050294337727,0.500664234338952));
#23002=DIRECTION('',(0.,1.,0.));
#23003=DIRECTION('center_axis',(0.3582068848149,0.554700196225404,-0.75099635150825));
#23004=DIRECTION('ref_axis',(-0.238804589876937,0.832050294337727,0.500664234338953));
#23005=DIRECTION('center_axis',(0.,1.,0.));
#23006=DIRECTION('ref_axis',(-6.82745422938049E-13,0.,1.));
#23007=DIRECTION('center_axis',(-0.75099635150825,0.554700196225404,0.3582068848149));
#23008=DIRECTION('ref_axis',(-0.500664234338953,-0.832050294337727,0.238804589876937));
#23009=DIRECTION('',(0.,-1.,0.));
#23010=DIRECTION('',(0.,1.,0.));
#23011=DIRECTION('',(0.,-1.,0.));
#23012=DIRECTION('center_axis',(0.902585284349861,0.,-0.430511096808295));
#23013=DIRECTION('ref_axis',(0.,-1.,0.));
#23014=DIRECTION('',(-0.430511096808721,0.,-0.902585284349657));
#23015=DIRECTION('',(0.430511096808721,0.,0.902585284349657));
#23016=DIRECTION('',(0.,1.,0.));
#23017=DIRECTION('center_axis',(-0.750996351508308,0.554700196225229,0.35820688481505));
#23018=DIRECTION('ref_axis',(0.430511096808295,-9.35899339744592E-17,0.902585284349861));
#23019=DIRECTION('',(-0.430511096808721,0.,-0.902585284349657));
#23020=DIRECTION('center_axis',(0.750996351508247,-0.554700196225413,-0.358206884814892));
#23021=DIRECTION('ref_axis',(0.500664234338957,0.832050294337721,-0.238804589876949));
#23022=DIRECTION('center_axis',(0.,1.,0.));
#23023=DIRECTION('ref_axis',(1.,0.,0.));
#23024=DIRECTION('',(0.902585284349657,0.,0.430511096808721));
#23025=DIRECTION('center_axis',(0.,-1.,0.));
#23026=DIRECTION('ref_axis',(7.19584204751227E-13,0.,-1.));
#23027=DIRECTION('center_axis',(0.35820688481505,0.554700196225229,-0.750996351508308));
#23028=DIRECTION('ref_axis',(-0.902585284349861,8.75902672829316E-17,-0.430511096808295));
#23029=DIRECTION('center_axis',(-0.358206884814892,-0.554700196225414,0.750996351508247));
#23030=DIRECTION('ref_axis',(0.23880458987695,-0.83205029433772,-0.500664234338957));
#23031=DIRECTION('',(-0.902585284349657,0.,-0.430511096808721));
#23032=DIRECTION('center_axis',(-0.430511096808295,0.,0.902585284349861));
#23033=DIRECTION('ref_axis',(0.,1.,0.));
#23034=DIRECTION('',(0.902585284349657,0.,0.430511096808721));
#23035=DIRECTION('',(0.,-1.,0.));
#23036=DIRECTION('center_axis',(0.35820688481505,-0.554700196225229,-0.750996351508308));
#23037=DIRECTION('ref_axis',(-4.41754862127715E-17,-0.804372725796521,0.594125001994256));
#23038=DIRECTION('',(-0.902585284349657,0.,-0.430511096808721));
#23039=DIRECTION('center_axis',(-0.358206884814892,0.554700196225413,0.750996351508247));
#23040=DIRECTION('ref_axis',(0.238804589876949,0.832050294337721,-0.500664234338957));
#23041=DIRECTION('center_axis',(0.,-1.,0.));
#23042=DIRECTION('ref_axis',(1.59744320089951E-16,0.,-1.));
#23043=DIRECTION('center_axis',(0.750996351508247,0.554700196225413,-0.358206884814892));
#23044=DIRECTION('ref_axis',(0.500664234338957,-0.832050294337721,-0.238804589876949));
#23045=DIRECTION('center_axis',(0.,-1.,0.));
#23046=DIRECTION('ref_axis',(7.19584204751227E-13,0.,-1.));
#23047=DIRECTION('center_axis',(0.,-1.,0.));
#23048=DIRECTION('ref_axis',(0.,0.,-1.));
#23049=DIRECTION('',(0.430511096808721,0.,0.902585284349657));
#23050=DIRECTION('center_axis',(-0.750996351508308,-0.554700196225229,0.35820688481505));
#23051=DIRECTION('ref_axis',(-0.594125001994256,0.804372725796521,4.34111046316595E-17));
#23052=DIRECTION('center_axis',(0.707106781186548,1.63268091856641E-16,
-0.707106781186547));
#23053=DIRECTION('ref_axis',(7.68102127765282E-32,-1.,-2.30895949806438E-16));
#23054=DIRECTION('',(-0.707106781186547,0.,-0.707106781186548));
#23055=DIRECTION('',(1.0001154479739E-12,-1.,-1.0001154479739E-12));
#23056=DIRECTION('',(-0.707106781186547,0.,-0.707106781186548));
#23057=DIRECTION('center_axis',(-0.707106781186547,0.,-0.707106781186548));
#23058=DIRECTION('ref_axis',(-0.707106781186548,0.,0.707106781186547));
#23059=DIRECTION('',(-0.707106781186547,0.,-0.707106781186548));
#23060=DIRECTION('center_axis',(-0.707106781186547,0.,-0.707106781186548));
#23061=DIRECTION('ref_axis',(-0.707106781186548,0.,0.707106781186547));
#23062=DIRECTION('center_axis',(-0.707106781186547,0.,-0.707106781186548));
#23063=DIRECTION('ref_axis',(0.707106781186548,0.,-0.707106781186547));
#23064=DIRECTION('center_axis',(-0.707106781186547,0.,-0.707106781186548));
#23065=DIRECTION('ref_axis',(0.707106781186548,0.,-0.707106781186547));
#23066=DIRECTION('',(-0.707106781186547,0.,-0.707106781186548));
#23067=DIRECTION('center_axis',(-0.707106781186548,8.16340459283203E-17,
0.707106781186547));
#23068=DIRECTION('ref_axis',(1.15447974903219E-16,1.,1.84458295290239E-31));
#23069=DIRECTION('',(1.00005772398645E-12,1.,-1.00005772398645E-12));
#23070=DIRECTION('center_axis',(0.,-1.,0.));
#23071=DIRECTION('ref_axis',(0.707106781186547,0.,0.707106781186548));
#23072=DIRECTION('center_axis',(-0.277744095478098,-0.554700196225389,0.784325130117969));
#23073=DIRECTION('ref_axis',(-0.185162730318571,0.832050294337737,0.522883420078948));
#23074=DIRECTION('center_axis',(0.,1.,0.));
#23075=DIRECTION('ref_axis',(0.707106781186547,0.,0.707106781186548));
#23076=DIRECTION('center_axis',(-0.277744095478098,-0.554700196225389,-0.784325130117969));
#23077=DIRECTION('ref_axis',(0.185162730318571,-0.832050294337737,0.522883420078948));
#23078=DIRECTION('',(0.,1.,0.));
#23079=DIRECTION('center_axis',(-0.277744095478098,0.554700196225389,-0.784325130117969));
#23080=DIRECTION('ref_axis',(0.185162730318571,0.832050294337737,0.522883420078948));
#23081=DIRECTION('center_axis',(0.,1.,0.));
#23082=DIRECTION('ref_axis',(0.707106781186547,0.,0.707106781186548));
#23083=DIRECTION('center_axis',(-0.277744095478098,0.554700196225389,0.784325130117969));
#23084=DIRECTION('ref_axis',(-0.185162730318571,-0.832050294337737,0.522883420078948));
#23085=DIRECTION('',(0.,-1.,0.));
#23086=DIRECTION('',(0.,1.,0.));
#23087=DIRECTION('',(0.,-1.,0.));
#23088=DIRECTION('center_axis',(0.333806859233771,0.,-0.942641491092178));
#23089=DIRECTION('ref_axis',(0.,-1.,0.));
#23090=DIRECTION('',(-0.942641491091975,0.,-0.333806859234345));
#23091=DIRECTION('',(0.942641491091975,0.,0.333806859234345));
#23092=DIRECTION('',(0.,1.,0.));
#23093=DIRECTION('center_axis',(-0.27774409547745,0.554700196225229,0.784325130118311));
#23094=DIRECTION('ref_axis',(0.894172998238226,0.447721620230319,1.29766088156978E-16));
#23095=DIRECTION('',(-0.942641491091975,0.,-0.333806859234345));
#23096=DIRECTION('center_axis',(0.277744095478133,-0.554700196225397,-0.78432513011795));
#23097=DIRECTION('ref_axis',(0.185162730318585,0.832050294337732,-0.522883420078951));
#23098=DIRECTION('center_axis',(0.,1.,0.));
#23099=DIRECTION('ref_axis',(1.,0.,0.));
#23100=DIRECTION('',(0.942641491091975,0.,-0.333806859234345));
#23101=DIRECTION('center_axis',(0.,-1.,0.));
#23102=DIRECTION('ref_axis',(-0.707106781186547,0.,-0.707106781186548));
#23103=DIRECTION('center_axis',(-0.27774409547745,0.554700196225229,-0.784325130118311));
#23104=DIRECTION('ref_axis',(-0.942641491092179,8.22449654774124E-17,0.333806859233771));
#23105=DIRECTION('center_axis',(0.277744095478132,-0.554700196225398,0.78432513011795));
#23106=DIRECTION('ref_axis',(-0.185162730318585,-0.832050294337731,-0.522883420078952));
#23107=DIRECTION('',(-0.942641491091975,0.,0.333806859234345));
#23108=DIRECTION('center_axis',(0.333806859233771,0.,0.942641491092178));
#23109=DIRECTION('ref_axis',(0.,-1.,0.));
#23110=DIRECTION('',(0.942641491091975,0.,-0.333806859234345));
#23111=DIRECTION('',(0.,-1.,0.));
#23112=DIRECTION('center_axis',(-0.27774409547745,-0.554700196225229,-0.784325130118311));
#23113=DIRECTION('ref_axis',(-1.53589745588664E-16,-0.816448204670702,0.577418677468947));
#23114=DIRECTION('',(-0.942641491091975,0.,0.333806859234345));
#23115=DIRECTION('center_axis',(0.277744095478133,0.554700196225397,0.78432513011795));
#23116=DIRECTION('ref_axis',(-0.185162730318585,0.832050294337732,-0.522883420078951));
#23117=DIRECTION('center_axis',(0.,-1.,0.));
#23118=DIRECTION('ref_axis',(-0.707106781186547,0.,-0.707106781186548));
#23119=DIRECTION('center_axis',(0.277744095478133,0.554700196225397,-0.78432513011795));
#23120=DIRECTION('ref_axis',(0.185162730318585,-0.832050294337732,-0.522883420078951));
#23121=DIRECTION('center_axis',(0.,-1.,0.));
#23122=DIRECTION('ref_axis',(-0.707106781186547,0.,-0.707106781186548));
#23123=DIRECTION('center_axis',(0.,-1.,0.));
#23124=DIRECTION('ref_axis',(0.,0.,-1.));
#23125=DIRECTION('',(0.942641491091975,0.,0.333806859234345));
#23126=DIRECTION('center_axis',(-0.27774409547745,-0.554700196225229,0.784325130118311));
#23127=DIRECTION('ref_axis',(-0.894172998238226,0.447721620230319,-1.29766088156978E-16));
#23128=DIRECTION('center_axis',(1.11022302462516E-16,1.63268091856641E-16,
-1.));
#23129=DIRECTION('ref_axis',(-1.,-1.12696337893758E-48,-1.11022302462516E-16));
#23130=DIRECTION('',(-1.,0.,-1.00011102230146E-12));
#23131=DIRECTION('',(9.99999999999E-13,-1.,-1.00016326809086E-12));
#23132=DIRECTION('',(-1.,0.,-1.00011102230146E-12));
#23133=DIRECTION('center_axis',(-1.,0.,-1.85037170770859E-16));
#23134=DIRECTION('ref_axis',(-1.85037170770859E-16,0.,1.));
#23135=DIRECTION('',(-1.,0.,-1.00011102230146E-12));
#23136=DIRECTION('center_axis',(-1.,0.,-6.66685170379299E-12));
#23137=DIRECTION('ref_axis',(-6.66685170379299E-12,0.,1.));
#23138=DIRECTION('center_axis',(-1.,0.,-2.77555756156289E-16));
#23139=DIRECTION('ref_axis',(2.77555756156289E-16,0.,-1.));
#23140=DIRECTION('center_axis',(-1.,0.,-6.66694422237838E-12));
#23141=DIRECTION('ref_axis',(6.66694422237838E-12,0.,-1.));
#23142=DIRECTION('center_axis',(-1.,0.,-6.66694422237838E-12));
#23143=DIRECTION('ref_axis',(6.66694422237838E-12,0.,-1.));
#23144=DIRECTION('center_axis',(-1.,0.,-6.66694422237838E-12));
#23145=DIRECTION('ref_axis',(6.66694422237838E-12,0.,-1.));
#23146=DIRECTION('',(-1.,0.,-1.00011102230146E-12));
#23147=DIRECTION('center_axis',(-9.0631997382929E-33,8.16340459283203E-17,
1.));
#23148=DIRECTION('ref_axis',(1.,1.11022302462516E-16,5.6348168946886E-49));
#23149=DIRECTION('',(9.99999999999E-13,1.,-1.00008163404493E-12));
#23150=DIRECTION('center_axis',(0.,1.,0.));
#23151=DIRECTION('ref_axis',(1.,0.,0.));
#23152=DIRECTION('',(1.00027992850901E-12,0.,-1.));
#23153=DIRECTION('',(-0.707106781186547,0.,-0.707106781186548));
#23154=DIRECTION('',(-1.,0.,-1.00027992850901E-12));
#23155=DIRECTION('',(-0.707106781186548,0.,0.707106781186547));
#23156=DIRECTION('',(1.00027992850901E-12,0.,1.));
#23157=DIRECTION('',(0.707106781186547,0.,0.707106781186548));
#23158=DIRECTION('',(1.,0.,1.00027992850901E-12));
#23159=DIRECTION('',(0.707106781186548,0.,-0.707106781186547));
#23160=DIRECTION('',(-1.00029133863849E-12,0.,1.));
#23161=DIRECTION('',(-0.707106781186548,0.,0.707106781186548));
#23162=DIRECTION('',(-1.,0.,0.));
#23163=DIRECTION('',(-0.707106781186548,0.,-0.707106781186547));
#23164=DIRECTION('',(1.00014566931874E-12,0.,-1.));
#23165=DIRECTION('',(0.707106781186547,0.,-0.707106781186548));
#23166=DIRECTION('',(1.,0.,0.));
#23167=DIRECTION('',(0.707106781186548,0.,0.707106781186548));
#23168=DIRECTION('center_axis',(-0.707106781186548,0.,0.707106781186547));
#23169=DIRECTION('ref_axis',(0.,1.,0.));
#23170=DIRECTION('',(0.,1.,0.));
#23171=DIRECTION('',(0.,-1.,0.));
#23172=DIRECTION('',(-0.707106781186547,0.,-0.707106781186548));
#23173=DIRECTION('center_axis',(-2.19351898461705E-47,7.8359970714266E-32,
1.));
#23174=DIRECTION('ref_axis',(1.,2.79928510006155E-16,7.56996450688685E-62));
#23175=DIRECTION('',(0.,1.,0.));
#23176=DIRECTION('',(-1.,0.,-1.00027992850901E-12));
#23177=DIRECTION('center_axis',(0.707106781186547,0.,0.707106781186548));
#23178=DIRECTION('ref_axis',(0.,-1.,0.));
#23179=DIRECTION('',(0.,1.,0.));
#23180=DIRECTION('',(0.,1.,0.));
#23181=DIRECTION('',(-0.707106781186548,0.,0.707106781186547));
#23182=DIRECTION('center_axis',(0.707106781186548,0.,-0.707106781186547));
#23183=DIRECTION('ref_axis',(0.,-1.,0.));
#23184=DIRECTION('',(0.,1.,0.));
#23185=DIRECTION('',(0.,1.,0.));
#23186=DIRECTION('',(0.,1.,0.));
#23187=DIRECTION('',(0.707106781186547,0.,0.707106781186548));
#23188=DIRECTION('center_axis',(2.79928510006155E-16,0.,-1.));
#23189=DIRECTION('ref_axis',(0.,-1.,0.));
#23190=DIRECTION('',(0.,1.,0.));
#23191=DIRECTION('',(1.,0.,1.00027992850901E-12));
#23192=DIRECTION('center_axis',(-0.707106781186547,0.,-0.707106781186548));
#23193=DIRECTION('ref_axis',(-0.707106781186548,0.,0.707106781186547));
#23194=DIRECTION('',(0.,1.,0.));
#23195=DIRECTION('',(0.707106781186548,0.,-0.707106781186547));
#23196=DIRECTION('center_axis',(-1.,0.,2.79928510006155E-16));
#23197=DIRECTION('ref_axis',(0.,1.,0.));
#23198=DIRECTION('',(-1.00027992850901E-12,0.,-1.));
#23199=DIRECTION('center_axis',(0.,-1.,0.));
#23200=DIRECTION('ref_axis',(0.,0.,-1.));
#23201=DIRECTION('',(1.,0.,1.00027755575516E-12));
#23202=DIRECTION('',(1.00027992850901E-12,1.00002114947192E-12,-1.));
#23203=DIRECTION('',(1.,0.,1.00027755575516E-12));
#23204=DIRECTION('',(-1.,0.,-1.00027992850901E-12));
#23205=DIRECTION('',(1.00029133863849E-12,0.,-1.));
#23206=DIRECTION('',(-0.707106781186548,0.,-0.707106781186548));
#23207=DIRECTION('',(-1.,0.,0.));
#23208=DIRECTION('',(-0.707106781186547,0.,0.707106781186548));
#23209=DIRECTION('',(-1.00014566931874E-12,0.,1.));
#23210=DIRECTION('',(0.707106781186548,0.,0.707106781186547));
#23211=DIRECTION('',(1.,0.,0.));
#23212=DIRECTION('',(0.707106781186548,0.,-0.707106781186548));
#23213=DIRECTION('',(1.00029133863849E-12,0.,-1.));
#23214=DIRECTION('',(1.,0.,1.00027992850901E-12));
#23215=DIRECTION('',(1.00027992850901E-12,0.,-1.));
#23216=DIRECTION('center_axis',(-0.707106781186548,0.,-0.707106781186548));
#23217=DIRECTION('ref_axis',(-0.707106781186548,0.,0.707106781186548));
#23218=DIRECTION('',(0.,1.,0.));
#23219=DIRECTION('',(0.,1.,0.));
#23220=DIRECTION('center_axis',(0.,0.,-1.));
#23221=DIRECTION('ref_axis',(0.,-1.,0.));
#23222=DIRECTION('',(0.,-1.,0.));
#23223=DIRECTION('center_axis',(0.707106781186547,0.,-0.707106781186548));
#23224=DIRECTION('ref_axis',(0.,-1.,0.));
#23225=DIRECTION('',(0.,1.,0.));
#23226=DIRECTION('center_axis',(1.,2.12195507149859E-32,3.0910375179476E-48));
#23227=DIRECTION('ref_axis',(6.6848796930149E-63,-1.45669319745051E-16,
1.));
#23228=DIRECTION('',(0.,1.,0.));
#23229=DIRECTION('center_axis',(0.707106781186548,0.,0.707106781186547));
#23230=DIRECTION('ref_axis',(0.,-1.,0.));
#23231=DIRECTION('',(0.,1.,0.));
#23232=DIRECTION('center_axis',(0.,0.,1.));
#23233=DIRECTION('ref_axis',(1.,0.,0.));
#23234=DIRECTION('',(0.,1.,0.));
#23235=DIRECTION('center_axis',(-0.707106781186548,0.,0.707106781186548));
#23236=DIRECTION('ref_axis',(0.,1.,0.));
#23237=DIRECTION('',(0.,1.,0.));
#23238=DIRECTION('center_axis',(0.,1.,0.));
#23239=DIRECTION('ref_axis',(1.,0.,0.));
#23240=DIRECTION('',(-1.00029133863849E-12,0.,1.));
#23241=DIRECTION('',(-1.,0.,0.));
#23242=DIRECTION('',(1.00027992850901E-12,0.,-1.));
#23243=DIRECTION('',(-1.,0.,0.));
#23244=DIRECTION('',(-1.00029133863849E-12,0.,1.));
#23245=DIRECTION('',(-1.00029133863849E-12,0.,1.));
#23246=DIRECTION('center_axis',(0.,1.5419764230905E-16,-1.));
#23247=DIRECTION('ref_axis',(-1.,0.,0.));
#23248=DIRECTION('',(-1.,0.,0.));
#23249=DIRECTION('',(9.99999999999E-13,-1.,-1.00024671622669E-12));
#23250=DIRECTION('',(1.,0.,1.00027755575516E-12));
#23251=DIRECTION('',(0.,1.,0.));
#23252=DIRECTION('',(0.,1.,0.));
#23253=DIRECTION('center_axis',(0.,0.,1.));
#23254=DIRECTION('ref_axis',(1.,0.,0.));
#23255=DIRECTION('',(1.,0.,1.00027755575516E-12));
#23256=DIRECTION('',(0.,1.,0.));
#23257=DIRECTION('',(-1.,0.,0.));
#23258=DIRECTION('',(0.,1.,0.));
#23259=DIRECTION('',(0.,-1.,0.));
#23260=DIRECTION('center_axis',(-1.,0.,-2.91338639490101E-16));
#23261=DIRECTION('ref_axis',(-2.91338639490101E-16,0.,1.));
#23262=DIRECTION('center_axis',(1.,7.70371977754894E-32,2.13821176807375E-47));
#23263=DIRECTION('ref_axis',(4.61864415153757E-62,-2.77555756156289E-16,
1.));
#23264=DIRECTION('',(-1.00027992850901E-12,0.,1.));
#23265=DIRECTION('',(-1.00027992850901E-12,-1.00015458001819E-12,1.));
#23266=DIRECTION('',(-1.00027992850901E-12,0.,1.));
#23267=DIRECTION('',(9.99999999999001E-13,-1.,-3.55964561715128E-12));
#23268=DIRECTION('',(-9.99999999999E-13,1.,1.00010573552515E-12));
#23269=DIRECTION('center_axis',(0.,1.,0.));
#23270=DIRECTION('ref_axis',(1.,0.,0.));
#23271=DIRECTION('',(1.00027992850901E-12,0.,-1.));
#23272=DIRECTION('',(1.,0.,1.00027755575516E-12));
#23273=DIRECTION('center_axis',(0.,1.,0.));
#23274=DIRECTION('ref_axis',(1.,0.,0.));
#23275=DIRECTION('',(1.00027992850901E-12,0.,-1.));
#23276=DIRECTION('',(1.,0.,1.00027755575516E-12));
#23277=DIRECTION('center_axis',(7.10444374761543E-28,-2.55964561715484E-12,
1.));
#23278=DIRECTION('ref_axis',(1.,2.77555756156289E-16,-3.7860081723633E-43));
#23279=DIRECTION('center_axis',(2.77555756156289E-16,1.05735526154777E-16,
-1.));
#23280=DIRECTION('ref_axis',(0.,-1.,-1.05735526154777E-16));
#23281=DIRECTION('center_axis',(-1.,0.,-2.91338639490101E-16));
#23282=DIRECTION('ref_axis',(-2.91338639490101E-16,0.,1.));
#23283=DIRECTION('center_axis',(1.,7.8359970714266E-32,2.19351898461705E-47));
#23284=DIRECTION('ref_axis',(-7.77876909732643E-62,-2.79928510006155E-16,
1.));
#23285=DIRECTION('center_axis',(0.,-1.,-1.2559626558816E-16));
#23286=DIRECTION('ref_axis',(0.,1.2559626558816E-16,-1.));
#23287=DIRECTION('',(-1.00027992850901E-12,-1.00012559626459E-12,1.));
#23288=DIRECTION('center_axis',(1.,7.8359970714266E-32,2.19351898461705E-47));
#23289=DIRECTION('ref_axis',(-7.77876909732643E-62,-2.79928510006155E-16,
1.));
#23290=DIRECTION('axis',(0.,0.,1.));
#23291=DIRECTION('refdir',(1.,0.,0.));
#23292=DIRECTION('center_axis',(6.65798752924967E-17,-1.,1.71022579061586E-31));
#23293=DIRECTION('ref_axis',(-0.345824623417469,-2.30249603002096E-17,0.938299168622762));
#23294=DIRECTION('',(-6.65798752924967E-17,1.,-1.71022579061586E-31));
#23295=DIRECTION('center_axis',(-6.65798752924967E-17,1.,-1.71022579061586E-31));
#23296=DIRECTION('ref_axis',(-0.345824623433441,-2.3024960301273E-17,0.938299168616875));
#23297=DIRECTION('',(6.65798752924967E-17,-1.,1.71022579061586E-31));
#23298=DIRECTION('center_axis',(6.65798752924967E-17,-1.,1.71022579061586E-31));
#23299=DIRECTION('ref_axis',(-0.345824623433441,-2.3024960301273E-17,0.938299168616875));
#23300=DIRECTION('center_axis',(6.65798752924967E-17,-1.,1.71022579061586E-31));
#23301=DIRECTION('ref_axis',(-0.473045086880378,-3.14952828922237E-17,0.881038220384528));
#23302=DIRECTION('',(-6.65798752924967E-17,1.,-1.71022579061586E-31));
#23303=DIRECTION('center_axis',(-6.65798752924967E-17,1.,-1.71022579061586E-31));
#23304=DIRECTION('ref_axis',(-0.473045086892459,-3.1495282893028E-17,0.881038220378041));
#23305=DIRECTION('',(6.65798752924967E-17,-1.,1.71022579061586E-31));
#23306=DIRECTION('center_axis',(6.65798752924967E-17,-1.,1.71022579061586E-31));
#23307=DIRECTION('ref_axis',(-0.473045086892459,-3.1495282893028E-17,0.881038220378041));
#23308=DIRECTION('center_axis',(6.65798752924967E-17,-1.,1.71022579061586E-31));
#23309=DIRECTION('ref_axis',(-0.591058265807973,-3.93525856280941E-17,0.80662886535263));
#23310=DIRECTION('',(-6.65798752924967E-17,1.,-1.71022579061586E-31));
#23311=DIRECTION('center_axis',(-6.65798752924967E-17,1.,-1.71022579061586E-31));
#23312=DIRECTION('ref_axis',(-0.591058265816149,-3.93525856286384E-17,0.806628865346639));
#23313=DIRECTION('',(6.65798752924967E-17,-1.,1.71022579061586E-31));
#23314=DIRECTION('center_axis',(6.65798752924967E-17,-1.,1.71022579061586E-31));
#23315=DIRECTION('ref_axis',(-0.591058265816149,-3.93525856286384E-17,0.806628865346639));
#23316=DIRECTION('center_axis',(6.65798752924967E-17,-1.,1.71022579061586E-31));
#23317=DIRECTION('ref_axis',(-0.697567167910428,-4.64439350476163E-17,0.716519396983379));
#23318=DIRECTION('',(-6.65798752924967E-17,1.,-1.71022579061586E-31));
#23319=DIRECTION('center_axis',(-6.65798752924967E-17,1.,-1.71022579061586E-31));
#23320=DIRECTION('ref_axis',(-0.697567167914987,-4.64439350479198E-17,0.716519396978941));
#23321=DIRECTION('',(6.65798752924967E-17,-1.,1.71022579061586E-31));
#23322=DIRECTION('center_axis',(6.65798752924967E-17,-1.,1.71022579061586E-31));
#23323=DIRECTION('ref_axis',(-0.697567167914987,-4.64439350479198E-17,0.716519396978941));
#23324=DIRECTION('center_axis',(6.65798752924967E-17,-1.,1.71022579061586E-31));
#23325=DIRECTION('ref_axis',(-0.790498718560399,-5.26313061006297E-17,0.61246369358058));
#23326=DIRECTION('',(-6.65798752924967E-17,1.,-1.71022579061586E-31));
#23327=DIRECTION('center_axis',(-6.65798752924967E-17,1.,-1.71022579061586E-31));
#23328=DIRECTION('ref_axis',(-0.790498718561909,-5.26313061007302E-17,0.612463693578632));
#23329=DIRECTION('',(6.65798752924967E-17,-1.,1.71022579061586E-31));
#23330=DIRECTION('center_axis',(6.65798752924967E-17,-1.,1.71022579061586E-31));
#23331=DIRECTION('ref_axis',(-0.790498718561909,-5.26313061007302E-17,0.612463693578632));
#23332=DIRECTION('center_axis',(6.65798752924967E-17,-1.,1.71022579061586E-31));
#23333=DIRECTION('ref_axis',(-0.868044110832557,-5.77942686476178E-17,0.496487081049362));
#23334=DIRECTION('',(-6.65798752924967E-17,1.,-1.71022579061586E-31));
#23335=DIRECTION('center_axis',(-6.65798752924967E-17,1.,-1.71022579061586E-31));
#23336=DIRECTION('ref_axis',(-0.868044110831822,-5.77942686475688E-17,0.496487081050647));
#23337=DIRECTION('',(6.65798752924967E-17,-1.,1.71022579061586E-31));
#23338=DIRECTION('center_axis',(6.65798752924967E-17,-1.,1.71022579061586E-31));
#23339=DIRECTION('ref_axis',(-0.868044110831822,-5.77942686475688E-17,0.496487081050647));
#23340=DIRECTION('center_axis',(6.65798752924967E-17,-1.,1.71022579061586E-31));
#23341=DIRECTION('ref_axis',(-0.928694011872901,-6.18323314953861E-17,0.370846912231201));
#23342=DIRECTION('',(-6.65798752924967E-17,1.,-1.71022579061586E-31));
#23343=DIRECTION('center_axis',(-6.65798752924967E-17,1.,-1.71022579061586E-31));
#23344=DIRECTION('ref_axis',(-0.9286940118709,-6.18323314952529E-17,0.370846912236213));
#23345=DIRECTION('',(6.65798752924967E-17,-1.,1.71022579061586E-31));
#23346=DIRECTION('center_axis',(6.65798752924967E-17,-1.,1.71022579061586E-31));
#23347=DIRECTION('ref_axis',(-0.9286940118709,-6.18323314952529E-17,0.370846912236213));
#23348=DIRECTION('center_axis',(6.65798752924967E-17,-1.,1.71022579061586E-31));
#23349=DIRECTION('ref_axis',(-0.97126794034592,-6.46668983438314E-17,0.237988630098571));
#23350=DIRECTION('',(-6.65798752924967E-17,1.,-1.71022579061586E-31));
#23351=DIRECTION('center_axis',(-6.65798752924967E-17,1.,-1.71022579061586E-31));
#23352=DIRECTION('ref_axis',(-0.971267940343728,-6.46668983436855E-17,0.237988630107515));
#23353=DIRECTION('',(6.65798752924967E-17,-1.,1.71022579061586E-31));
#23354=DIRECTION('center_axis',(6.65798752924967E-17,-1.,1.71022579061586E-31));
#23355=DIRECTION('ref_axis',(-0.971267940343728,-6.46668983436855E-17,0.237988630107515));
#23356=DIRECTION('center_axis',(6.65798752924967E-17,-1.,1.71022579061586E-31));
#23357=DIRECTION('ref_axis',(-0.994937243161013,-6.62427975735207E-17,0.100498169989126));
#23358=DIRECTION('',(-6.65798752924967E-17,1.,-1.71022579061586E-31));
#23359=DIRECTION('center_axis',(-6.65798752924967E-17,1.,-1.71022579061586E-31));
#23360=DIRECTION('ref_axis',(-0.994937243159722,-6.62427975734348E-17,0.100498170001902));
#23361=DIRECTION('',(6.65798752924967E-17,-1.,1.71022579061586E-31));
#23362=DIRECTION('center_axis',(6.65798752924967E-17,-1.,1.71022579061586E-31));
#23363=DIRECTION('ref_axis',(-0.994937243159722,-6.62427975734348E-17,0.100498170001902));
#23364=DIRECTION('center_axis',(6.65798752924967E-17,-1.,1.71022579061586E-31));
#23365=DIRECTION('ref_axis',(-0.999241224262317,-6.65293560985068E-17,-0.0389483726841831));
#23366=DIRECTION('',(-6.65798752924967E-17,1.,-1.71022579061586E-31));
#23367=DIRECTION('center_axis',(-6.65798752924967E-17,1.,-1.71022579061586E-31));
#23368=DIRECTION('ref_axis',(-0.999241224262949,-6.65293560985489E-17,-0.038948372667972));
#23369=DIRECTION('',(6.65798752924967E-17,-1.,1.71022579061586E-31));
#23370=DIRECTION('center_axis',(6.65798752924967E-17,-1.,1.71022579061586E-31));
#23371=DIRECTION('ref_axis',(-0.999241224262949,-6.65293560985489E-17,-0.038948372667972));
#23372=DIRECTION('center_axis',(6.65798752924967E-17,-1.,1.71022579061586E-31));
#23373=DIRECTION('ref_axis',(-0.984096111553401,-6.55209963830564E-17,-0.177636829586311));
#23374=DIRECTION('',(-6.65798752924967E-17,1.,-1.71022579061586E-31));
#23375=DIRECTION('center_axis',(-6.65798752924967E-17,1.,-1.71022579061586E-31));
#23376=DIRECTION('ref_axis',(-0.984096111556828,-6.55209963832845E-17,-0.177636829567328));
#23377=DIRECTION('',(6.65798752924967E-17,-1.,1.71022579061586E-31));
#23378=DIRECTION('center_axis',(6.65798752924967E-17,-1.,1.71022579061586E-31));
#23379=DIRECTION('ref_axis',(-0.984096111556828,-6.55209963832845E-17,-0.177636829567328));
#23380=DIRECTION('center_axis',(6.65798752924967E-17,-1.,1.71022579061586E-31));
#23381=DIRECTION('ref_axis',(-0.949796687425834,-6.32373450020385E-17,-0.312867787659441));
#23382=DIRECTION('',(-6.65798752924967E-17,1.,-1.71022579061586E-31));
#23383=DIRECTION('center_axis',(-6.65798752924967E-17,1.,-1.71022579061586E-31));
#23384=DIRECTION('ref_axis',(-0.949796687420265,-6.32373450016678E-17,-0.312867787676347));
#23385=DIRECTION('',(6.65798752924967E-17,-1.,1.71022579061586E-31));
#23386=DIRECTION('center_axis',(6.65798752924967E-17,-1.,1.71022579061586E-31));
#23387=DIRECTION('ref_axis',(-0.949796687420265,-6.32373450016678E-17,-0.312867787676347));
#23388=DIRECTION('center_axis',(6.65798752924967E-17,-1.,1.71022579061586E-31));
#23389=DIRECTION('ref_axis',(-0.897010551155241,-5.97228506319698E-17,-0.442009130127614));
#23390=DIRECTION('',(-6.65798752924967E-17,1.,-1.71022579061586E-31));
#23391=DIRECTION('center_axis',(-6.65798752924967E-17,1.,-1.71022579061586E-31));
#23392=DIRECTION('ref_axis',(-0.897010551148803,-5.97228506315411E-17,-0.442009130140681));
#23393=DIRECTION('',(6.65798752924967E-17,-1.,1.71022579061586E-31));
#23394=DIRECTION('center_axis',(6.65798752924967E-17,-1.,1.71022579061586E-31));
#23395=DIRECTION('ref_axis',(-0.897010551148803,-5.97228506315411E-17,-0.442009130140681));
#23396=DIRECTION('center_axis',(6.65798752924967E-17,-1.,1.71022579061586E-31));
#23397=DIRECTION('ref_axis',(-0.826765124840791,-5.50459189080855E-17,-0.562547267655786));
#23398=DIRECTION('',(-6.65798752924967E-17,1.,-1.71022579061586E-31));
#23399=DIRECTION('center_axis',(-6.65798752924967E-17,1.,-1.71022579061586E-31));
#23400=DIRECTION('ref_axis',(-0.826765124834574,-5.50459189076715E-17,-0.562547267664923));
#23401=DIRECTION('',(6.65798752924967E-17,-1.,1.71022579061586E-31));
#23402=DIRECTION('center_axis',(6.65798752924967E-17,-1.,1.71022579061586E-31));
#23403=DIRECTION('ref_axis',(-0.826765124834574,-5.50459189076715E-17,-0.562547267664923));
#23404=DIRECTION('center_axis',(6.65798752924967E-17,-1.,1.71022579061586E-31));
#23405=DIRECTION('ref_axis',(-0.740427655802706,-4.929758098646E-17,-0.672136062507071));
#23406=DIRECTION('',(-6.65798752924967E-17,1.,-1.71022579061586E-31));
#23407=DIRECTION('center_axis',(-6.65798752924967E-17,1.,-1.71022579061586E-31));
#23408=DIRECTION('ref_axis',(-0.740427655797785,-4.92975809861323E-17,-0.672136062512493));
#23409=DIRECTION('',(6.65798752924967E-17,-1.,1.71022579061586E-31));
#23410=DIRECTION('center_axis',(6.65798752924967E-17,-1.,1.71022579061586E-31));
#23411=DIRECTION('ref_axis',(-0.740427655797785,-4.92975809861323E-17,-0.672136062512493));
#23412=DIRECTION('center_axis',(6.65798752924967E-17,-1.,1.71022579061586E-31));
#23413=DIRECTION('ref_axis',(-0.639678604668397,-4.25897217261003E-17,-0.768642493445095));
#23414=DIRECTION('',(-6.65798752924967E-17,1.,-1.71022579061586E-31));
#23415=DIRECTION('center_axis',(-6.65798752924967E-17,1.,-1.71022579061586E-31));
#23416=DIRECTION('ref_axis',(-0.639678604665747,-4.25897217259239E-17,-0.7686424934473));
#23417=DIRECTION('',(6.65798752924967E-17,-1.,1.71022579061586E-31));
#23418=DIRECTION('center_axis',(6.65798752924967E-17,-1.,1.71022579061586E-31));
#23419=DIRECTION('ref_axis',(-0.639678604665747,-4.25897217259239E-17,-0.7686424934473));
#23420=DIRECTION('center_axis',(6.65798752924967E-17,-1.,1.71022579061586E-31));
#23421=DIRECTION('ref_axis',(-0.526478937117844,-3.50529019774324E-17,-0.850188172566088));
#23422=DIRECTION('',(-6.65798752924967E-17,1.,-1.71022579061586E-31));
#23423=DIRECTION('center_axis',(-6.65798752924967E-17,1.,-1.71022579061586E-31));
#23424=DIRECTION('ref_axis',(-0.526478937118264,-3.50529019774604E-17,-0.850188172565828));
#23425=DIRECTION('',(6.65798752924967E-17,-1.,1.71022579061586E-31));
#23426=DIRECTION('center_axis',(6.65798752924967E-17,-1.,1.71022579061586E-31));
#23427=DIRECTION('ref_axis',(-0.526478937118264,-3.50529019774604E-17,-0.850188172565828));
#23428=DIRECTION('center_axis',(6.65798752924967E-17,-1.,1.71022579061586E-31));
#23429=DIRECTION('ref_axis',(-0.403031955917209,-2.6833817363859E-17,-0.915185905982795));
#23430=DIRECTION('',(-6.65798752924967E-17,1.,-1.71022579061586E-31));
#23431=DIRECTION('center_axis',(-6.65798752924967E-17,1.,-1.71022579061586E-31));
#23432=DIRECTION('ref_axis',(-0.403031955921259,-2.68338173641286E-17,-0.915185905981011));
#23433=DIRECTION('',(6.65798752924967E-17,-1.,1.71022579061586E-31));
#23434=DIRECTION('center_axis',(6.65798752924967E-17,-1.,1.71022579061586E-31));
#23435=DIRECTION('ref_axis',(-0.403031955921259,-2.68338173641286E-17,-0.915185905981011));
#23436=DIRECTION('center_axis',(6.65798752924967E-17,-1.,1.71022579061586E-31));
#23437=DIRECTION('ref_axis',(-0.2717404161367,-1.80924430183128E-17,-0.962370586748085));
#23438=DIRECTION('',(-6.65798752924967E-17,1.,-1.71022579061586E-31));
#23439=DIRECTION('center_axis',(-6.65798752924967E-17,1.,-1.71022579061586E-31));
#23440=DIRECTION('ref_axis',(-0.271740416144659,-1.80924430188427E-17,-0.962370586745838));
#23441=DIRECTION('',(6.65798752924967E-17,-1.,1.71022579061586E-31));
#23442=DIRECTION('center_axis',(6.65798752924967E-17,-1.,1.71022579061586E-31));
#23443=DIRECTION('ref_axis',(-0.271740416144659,-1.80924430188427E-17,-0.962370586745838));
#23444=DIRECTION('center_axis',(6.65798752924967E-17,-1.,1.71022579061586E-31));
#23445=DIRECTION('ref_axis',(-0.135159758256232,-8.9989198492641E-18,-0.990823818722641));
#23446=DIRECTION('',(-6.65798752924967E-17,1.,-1.71022579061586E-31));
#23447=DIRECTION('center_axis',(-6.65798752924967E-17,1.,-1.71022579061586E-31));
#23448=DIRECTION('ref_axis',(-0.135159758268076,-8.99891985005266E-18,-0.990823818721025));
#23449=DIRECTION('',(6.65798752924967E-17,-1.,1.71022579061586E-31));
#23450=DIRECTION('center_axis',(6.65798752924967E-17,-1.,1.71022579061586E-31));
#23451=DIRECTION('ref_axis',(-0.135159758268076,-8.99891985005266E-18,-0.990823818721025));
#23452=DIRECTION('center_axis',(6.65798752924967E-17,-1.,1.71022579061586E-31));
#23453=DIRECTION('ref_axis',(0.00405163057674682,2.69757058530899E-19,-0.99999179211115));
#23454=DIRECTION('',(-6.65798752924967E-17,1.,-1.71022579061586E-31));
#23455=DIRECTION('center_axis',(-6.65798752924967E-17,1.,-1.71022579061586E-31));
#23456=DIRECTION('ref_axis',(0.00405163056134247,2.69757057505279E-19,-0.999991792111212));
#23457=DIRECTION('',(6.65798752924967E-17,-1.,1.71022579061586E-31));
#23458=DIRECTION('center_axis',(6.65798752924967E-17,-1.,1.71022579061586E-31));
#23459=DIRECTION('ref_axis',(0.00405163056134247,2.69757057505279E-19,-0.999991792111212));
#23460=DIRECTION('center_axis',(6.65798752924967E-17,-1.,1.71022579061586E-31));
#23461=DIRECTION('ref_axis',(0.143184159029212,9.53318345202578E-18,-0.98969606274002));
#23462=DIRECTION('',(-6.65798752924967E-17,1.,-1.71022579061586E-31));
#23463=DIRECTION('center_axis',(-6.65798752924967E-17,1.,-1.71022579061586E-31));
#23464=DIRECTION('ref_axis',(0.143184159010847,9.53318345080304E-18,-0.989696062742677));
#23465=DIRECTION('',(6.65798752924967E-17,-1.,1.71022579061586E-31));
#23466=DIRECTION('center_axis',(6.65798752924967E-17,-1.,1.71022579061586E-31));
#23467=DIRECTION('ref_axis',(0.143184159010847,9.53318345080304E-18,-0.989696062742677));
#23468=DIRECTION('center_axis',(6.65798752924967E-17,-1.,1.71022579061586E-31));
#23469=DIRECTION('ref_axis',(0.27952977069574,1.86110572734624E-17,-0.960137025270241));
#23470=DIRECTION('',(-6.65798752924967E-17,1.,-1.71022579061586E-31));
#23471=DIRECTION('center_axis',(-6.65798752924967E-17,1.,-1.71022579061586E-31));
#23472=DIRECTION('ref_axis',(0.279529770713557,1.86110572746487E-17,-0.960137025265054));
#23473=DIRECTION('',(6.65798752924967E-17,-1.,1.71022579061586E-31));
#23474=DIRECTION('center_axis',(6.65798752924967E-17,-1.,1.71022579061586E-31));
#23475=DIRECTION('ref_axis',(0.279529770713557,1.86110572746487E-17,-0.960137025265054));
#23476=DIRECTION('center_axis',(6.65798752924967E-17,-1.,1.71022579061586E-31));
#23477=DIRECTION('ref_axis',(0.410434653336076,2.73266880348349E-17,-0.911890012743256));
#23478=DIRECTION('',(-6.65798752924967E-17,1.,-1.71022579061586E-31));
#23479=DIRECTION('center_axis',(-6.65798752924967E-17,1.,-1.71022579061586E-31));
#23480=DIRECTION('ref_axis',(0.410434653350123,2.73266880357702E-17,-0.911890012736933));
#23481=DIRECTION('',(6.65798752924967E-17,-1.,1.71022579061586E-31));
#23482=DIRECTION('center_axis',(6.65798752924967E-17,-1.,1.71022579061586E-31));
#23483=DIRECTION('ref_axis',(0.410434653350123,2.73266880357702E-17,-0.911890012736933));
#23484=DIRECTION('center_axis',(6.65798752924967E-17,-1.,1.71022579061586E-31));
#23485=DIRECTION('ref_axis',(0.533350892311725,3.55104358972563E-17,-0.845894098377738));
#23486=DIRECTION('',(-6.65798752924967E-17,1.,-1.71022579061586E-31));
#23487=DIRECTION('center_axis',(-6.65798752924967E-17,1.,-1.71022579061586E-31));
#23488=DIRECTION('ref_axis',(0.533350892321836,3.55104358979295E-17,-0.845894098371363));
#23489=DIRECTION('',(6.65798752924967E-17,-1.,1.71022579061586E-31));
#23490=DIRECTION('center_axis',(6.65798752924967E-17,-1.,1.71022579061586E-31));
#23491=DIRECTION('ref_axis',(0.533350892321836,3.55104358979295E-17,-0.845894098371363));
#23492=DIRECTION('center_axis',(6.65798752924967E-17,-1.,1.71022579061586E-31));
#23493=DIRECTION('ref_axis',(0.645886062846174,4.30030135174598E-17,-0.763433817577574));
#23494=DIRECTION('',(-6.65798752924967E-17,1.,-1.71022579061586E-31));
#23495=DIRECTION('center_axis',(-6.65798752924967E-17,1.,-1.71022579061586E-31));
#23496=DIRECTION('ref_axis',(0.645886062852486,4.30030135178801E-17,-0.763433817572233));
#23497=DIRECTION('',(6.65798752924967E-17,-1.,1.71022579061586E-31));
#23498=DIRECTION('center_axis',(6.65798752924967E-17,-1.,1.71022579061586E-31));
#23499=DIRECTION('ref_axis',(0.645886062852486,4.30030135178801E-17,-0.763433817572233));
#23500=DIRECTION('center_axis',(6.65798752924967E-17,-1.,1.71022579061586E-31));
#23501=DIRECTION('ref_axis',(0.745849795851828,4.96585863947487E-17,-0.666114165911359));
#23502=DIRECTION('',(-6.65798752924967E-17,1.,-1.71022579061586E-31));
#23503=DIRECTION('center_axis',(-6.65798752924967E-17,1.,-1.71022579061586E-31));
#23504=DIRECTION('ref_axis',(0.745849795854776,4.9658586394945E-17,-0.66611416590806));
#23505=DIRECTION('',(6.65798752924967E-17,-1.,1.71022579061586E-31));
#23506=DIRECTION('center_axis',(6.65798752924967E-17,-1.,1.71022579061586E-31));
#23507=DIRECTION('ref_axis',(0.745849795854776,4.9658586394945E-17,-0.66611416590806));
#23508=DIRECTION('center_axis',(6.65798752924967E-17,-1.,1.71022579061586E-31));
#23509=DIRECTION('ref_axis',(0.831296410972796,5.53476113736688E-17,-0.555829359699313));
#23510=DIRECTION('',(-6.65798752924967E-17,1.,-1.71022579061586E-31));
#23511=DIRECTION('center_axis',(-6.65798752924967E-17,1.,-1.71022579061586E-31));
#23512=DIRECTION('ref_axis',(0.83129641097307,5.5347611373687E-17,-0.555829359698903));
#23513=DIRECTION('',(6.65798752924967E-17,-1.,1.71022579061586E-31));
#23514=DIRECTION('center_axis',(6.65798752924967E-17,-1.,1.71022579061586E-31));
#23515=DIRECTION('ref_axis',(0.83129641097307,5.5347611373687E-17,-0.555829359698903));
#23516=DIRECTION('center_axis',(6.65798752924967E-17,-1.,1.71022579061586E-31));
#23517=DIRECTION('ref_axis',(0.900562787039831,5.99593580541751E-17,-0.434725967247245));
#23518=DIRECTION('',(-6.65798752924967E-17,1.,-1.71022579061586E-31));
#23519=DIRECTION('center_axis',(-6.65798752924967E-17,1.,-1.71022579061586E-31));
#23520=DIRECTION('ref_axis',(0.900562787038332,5.99593580540753E-17,-0.434725967250349));
#23521=DIRECTION('',(6.65798752924967E-17,-1.,1.71022579061586E-31));
#23522=DIRECTION('center_axis',(6.65798752924967E-17,-1.,1.71022579061586E-31));
#23523=DIRECTION('ref_axis',(0.900562787038332,5.99593580540753E-17,-0.434725967250349));
#23524=DIRECTION('center_axis',(6.65798752924967E-17,-1.,1.71022579061586E-31));
#23525=DIRECTION('ref_axis',(0.952300732832122,6.34040640329159E-17,-0.305161128336168));
#23526=DIRECTION('',(-6.65798752924967E-17,1.,-1.71022579061586E-31));
#23527=DIRECTION('center_axis',(-6.65798752924967E-17,1.,-1.71022579061586E-31));
#23528=DIRECTION('ref_axis',(0.952300732829888,6.34040640327671E-17,-0.30516112834314));
#23529=DIRECTION('',(6.65798752924967E-17,-1.,1.71022579061586E-31));
#23530=DIRECTION('center_axis',(6.65798752924967E-17,-1.,1.71022579061586E-31));
#23531=DIRECTION('ref_axis',(0.952300732829888,6.34040640327671E-17,-0.30516112834314));
#23532=DIRECTION('center_axis',(6.65798752924967E-17,-1.,1.71022579061586E-31));
#23533=DIRECTION('ref_axis',(0.985503228085865,6.56146820263098E-17,-0.169656675177667));
#23534=DIRECTION('',(-6.65798752924967E-17,1.,-1.71022579061586E-31));
#23535=DIRECTION('center_axis',(-6.65798752924967E-17,1.,-1.71022579061586E-31));
#23536=DIRECTION('ref_axis',(0.985503228083989,6.56146820261849E-17,-0.169656675188558));
#23537=DIRECTION('',(6.65798752924967E-17,-1.,1.71022579061586E-31));
#23538=DIRECTION('center_axis',(6.65798752924967E-17,-1.,1.71022579061586E-31));
#23539=DIRECTION('ref_axis',(0.985503228083989,6.56146820261849E-17,-0.169656675188558));
#23540=DIRECTION('center_axis',(6.65798752924967E-17,-1.,1.71022579061586E-31));
#23541=DIRECTION('ref_axis',(0.999524023998223,6.65481848696562E-17,-0.0308500478184399));
#23542=DIRECTION('',(-6.65798752924967E-17,1.,-1.71022579061586E-31));
#23543=DIRECTION('center_axis',(-6.65798752924967E-17,1.,-1.71022579061586E-31));
#23544=DIRECTION('ref_axis',(0.999524023997774,6.65481848696262E-17,-0.0308500478330001));
#23545=DIRECTION('',(6.65798752924967E-17,-1.,1.71022579061586E-31));
#23546=DIRECTION('center_axis',(6.65798752924967E-17,-1.,1.71022579061586E-31));
#23547=DIRECTION('ref_axis',(0.999524023997774,6.65481848696262E-17,-0.0308500478330001));
#23548=DIRECTION('center_axis',(6.65798752924967E-17,-1.,1.71022579061586E-31));
#23549=DIRECTION('ref_axis',(0.994090221725182,6.6186402991953E-17,0.108557040630164));
#23550=DIRECTION('',(-6.65798752924967E-17,1.,-1.71022579061586E-31));
#23551=DIRECTION('center_axis',(-6.65798752924967E-17,1.,-1.71022579061586E-31));
#23552=DIRECTION('ref_axis',(0.994090221727114,6.61864029920817E-17,0.108557040612469));
#23553=DIRECTION('',(6.65798752924967E-17,-1.,1.71022579061586E-31));
#23554=DIRECTION('center_axis',(6.65798752924967E-17,-1.,1.71022579061586E-31));
#23555=DIRECTION('ref_axis',(0.994090221727114,6.61864029920817E-17,0.108557040612469));
#23556=DIRECTION('center_axis',(6.65798752924967E-17,-1.,1.71022579061586E-31));
#23557=DIRECTION('ref_axis',(0.969307584047127,6.4536378065929E-17,0.245851189764706));
#23558=DIRECTION('',(-6.65798752924967E-17,1.,-1.71022579061586E-31));
#23559=DIRECTION('center_axis',(-6.65798752924967E-17,1.,-1.71022579061586E-31));
#23560=DIRECTION('ref_axis',(0.969307584042385,6.45363780656133E-17,0.245851189783404));
#23561=DIRECTION('',(6.65798752924967E-17,-1.,1.71022579061586E-31));
#23562=DIRECTION('center_axis',(6.65798752924967E-17,-1.,1.71022579061586E-31));
#23563=DIRECTION('ref_axis',(0.969307584042385,6.45363780656133E-17,0.245851189783404));
#23564=DIRECTION('center_axis',(6.65798752924967E-17,-1.,1.71022579061586E-31));
#23565=DIRECTION('ref_axis',(0.925658476816631,6.16302259498938E-17,0.37836012514206));
#23566=DIRECTION('',(-6.65798752924967E-17,1.,-1.71022579061586E-31));
#23567=DIRECTION('center_axis',(-6.65798752924967E-17,1.,-1.71022579061586E-31));
#23568=DIRECTION('ref_axis',(0.925658476810492,6.16302259494851E-17,0.378360125157078));
#23569=DIRECTION('',(6.65798752924967E-17,-1.,1.71022579061586E-31));
#23570=DIRECTION('center_axis',(6.65798752924967E-17,-1.,1.71022579061586E-31));
#23571=DIRECTION('ref_axis',(0.925658476810492,6.16302259494851E-17,0.378360125157078));
#23572=DIRECTION('center_axis',(6.65798752924967E-17,-1.,1.71022579061586E-31));
#23573=DIRECTION('ref_axis',(0.86399248025581,5.75245115890868E-17,0.503504711061788));
#23574=DIRECTION('',(-6.65798752924967E-17,1.,-1.71022579061586E-31));
#23575=DIRECTION('center_axis',(-6.65798752924967E-17,1.,-1.71022579061586E-31));
#23576=DIRECTION('ref_axis',(0.863992480249344,5.75245115886563E-17,0.503504711072882));
#23577=DIRECTION('',(6.65798752924967E-17,-1.,1.71022579061586E-31));
#23578=DIRECTION('center_axis',(6.65798752924967E-17,-1.,1.71022579061586E-31));
#23579=DIRECTION('ref_axis',(0.863992480249344,5.75245115886563E-17,0.503504711072882));
#23580=DIRECTION('center_axis',(6.65798752924967E-17,-1.,1.71022579061586E-31));
#23581=DIRECTION('ref_axis',(0.785509852843689,5.22991480433604E-17,0.618849150508818));
#23582=DIRECTION('',(-6.65798752924967E-17,1.,-1.71022579061586E-31));
#23583=DIRECTION('center_axis',(-6.65798752924967E-17,1.,-1.71022579061586E-31));
#23584=DIRECTION('ref_axis',(0.78550985283799,5.22991480429809E-17,0.618849150516052));
#23585=DIRECTION('',(6.65798752924967E-17,-1.,1.71022579061586E-31));
#23586=DIRECTION('center_axis',(6.65798752924967E-17,-1.,1.71022579061586E-31));
#23587=DIRECTION('ref_axis',(0.78550985283799,5.22991480429809E-17,0.618849150516052));
#23588=DIRECTION('center_axis',(6.65798752924967E-17,-1.,1.71022579061586E-31));
#23589=DIRECTION('ref_axis',(0.691738169650181,4.60558410703691E-17,0.72214839517167));
#23590=DIRECTION('',(-6.65798752924967E-17,1.,-1.71022579061586E-31));
#23591=DIRECTION('center_axis',(-6.65798752924967E-17,1.,-1.71022579061586E-31));
#23592=DIRECTION('ref_axis',(0.691738169646283,4.60558410701096E-17,0.722148395175403));
#23593=DIRECTION('',(6.65798752924967E-17,-1.,1.71022579061586E-31));
#23594=DIRECTION('center_axis',(6.65798752924967E-17,-1.,1.71022579061586E-31));
#23595=DIRECTION('ref_axis',(0.691738169646283,4.60558410701096E-17,0.722148395175403));
#23596=DIRECTION('center_axis',(6.65798752924967E-17,-1.,1.71022579061586E-31));
#23597=DIRECTION('ref_axis',(0.584502589824937,3.89161095386858E-17,0.811391842754129));
#23598=DIRECTION('',(-6.65798752924967E-17,1.,-1.71022579061586E-31));
#23599=DIRECTION('center_axis',(-6.65798752924967E-17,1.,-1.71022579061586E-31));
#23600=DIRECTION('ref_axis',(0.584502589823736,3.89161095386059E-17,0.811391842754994));
#23601=DIRECTION('',(6.65798752924967E-17,-1.,1.71022579061586E-31));
#23602=DIRECTION('center_axis',(6.65798752924967E-17,-1.,1.71022579061586E-31));
#23603=DIRECTION('ref_axis',(0.584502589823736,3.89161095386059E-17,0.811391842754994));
#23604=DIRECTION('center_axis',(6.65798752924967E-17,-1.,1.71022579061586E-31));
#23605=DIRECTION('ref_axis',(0.465890331950592,3.10189202012505E-17,0.884842471061921));
#23606=DIRECTION('',(-6.65798752924967E-17,1.,-1.71022579061586E-31));
#23607=DIRECTION('center_axis',(-6.65798752924967E-17,1.,-1.71022579061586E-31));
#23608=DIRECTION('ref_axis',(0.465890331952774,3.10189202013957E-17,0.884842471060773));
#23609=DIRECTION('',(6.65798752924967E-17,-1.,1.71022579061586E-31));
#23610=DIRECTION('center_axis',(6.65798752924967E-17,-1.,1.71022579061586E-31));
#23611=DIRECTION('ref_axis',(0.465890331952774,3.10189202013957E-17,0.884842471060773));
#23612=DIRECTION('center_axis',(6.65798752924967E-17,-1.,1.71022579061586E-31));
#23613=DIRECTION('ref_axis',(0.338210048707227,2.25179828655966E-17,0.941070647163886));
#23614=DIRECTION('',(-6.65798752924967E-17,1.,-1.71022579061586E-31));
#23615=DIRECTION('center_axis',(-6.65798752924967E-17,1.,-1.71022579061586E-31));
#23616=DIRECTION('ref_axis',(0.338210048713215,2.25179828659953E-17,0.941070647161734));
#23617=DIRECTION('',(6.65798752924967E-17,-1.,1.71022579061586E-31));
#23618=DIRECTION('center_axis',(6.65798752924967E-17,-1.,1.71022579061586E-31));
#23619=DIRECTION('ref_axis',(0.338210048713215,2.25179828659953E-17,0.941070647161734));
#23620=DIRECTION('center_axis',(6.65798752924967E-17,-1.,1.71022579061586E-31));
#23621=DIRECTION('ref_axis',(0.203946891574005,1.35787586072898E-17,0.978981953570801));
#23622=DIRECTION('',(-6.65798752924967E-17,1.,-1.71022579061586E-31));
#23623=DIRECTION('center_axis',(-6.65798752924967E-17,1.,-1.71022579061586E-31));
#23624=DIRECTION('ref_axis',(0.203946891583929,1.35787586079505E-17,0.978981953568733));
#23625=DIRECTION('',(6.65798752924967E-17,-1.,1.71022579061586E-31));
#23626=DIRECTION('center_axis',(6.65798752924967E-17,-1.,1.71022579061586E-31));
#23627=DIRECTION('ref_axis',(0.203946891583929,1.35787586079505E-17,0.978981953568733));
#23628=DIRECTION('center_axis',(6.65798752924967E-17,-1.,1.71022579061586E-31));
#23629=DIRECTION('ref_axis',(0.0657141401824452,4.37523925830102E-18,0.997838489826927));
#23630=DIRECTION('',(-6.65798752924967E-17,1.,-1.71022579061586E-31));
#23631=DIRECTION('center_axis',(-6.65798752924967E-17,1.,-1.71022579061586E-31));
#23632=DIRECTION('ref_axis',(0.0657141401961282,4.37523925921203E-18,0.997838489826026));
#23633=DIRECTION('',(6.65798752924967E-17,-1.,1.71022579061586E-31));
#23634=DIRECTION('center_axis',(6.65798752924967E-17,-1.,1.71022579061586E-31));
#23635=DIRECTION('ref_axis',(0.0657141401961282,4.37523925921203E-18,0.997838489826026));
#23636=DIRECTION('center_axis',(6.65798752924967E-17,-1.,1.71022579061586E-31));
#23637=DIRECTION('ref_axis',(-0.0737976621990395,-4.91343914608968E-18,
0.997273234903031));
#23638=DIRECTION('',(-6.65798752924967E-17,1.,-1.71022579061586E-31));
#23639=DIRECTION('center_axis',(-6.65798752924967E-17,1.,-1.71022579061586E-31));
#23640=DIRECTION('ref_axis',(-0.073797662182064,-4.91343914495945E-18,0.997273234904287));
#23641=DIRECTION('',(6.65798752924967E-17,-1.,1.71022579061586E-31));
#23642=DIRECTION('center_axis',(6.65798752924967E-17,-1.,1.71022579061586E-31));
#23643=DIRECTION('ref_axis',(-0.073797662182064,-4.91343914495945E-18,0.997273234904287));
#23644=DIRECTION('center_axis',(6.65798752924967E-17,-1.,1.71022579061586E-31));
#23645=DIRECTION('ref_axis',(0.97729719084324,6.50683250900503E-17,0.211873077029416));
#23646=DIRECTION('center_axis',(-6.65798752924967E-17,1.,-1.71022579061586E-31));
#23647=DIRECTION('ref_axis',(-0.211873077029416,-1.41064830464559E-17,0.97729719084324));
#23648=DIRECTION('center_axis',(6.65798752924967E-17,-1.,1.71022579061586E-31));
#23649=DIRECTION('ref_axis',(-0.211873077029416,-1.41064830464559E-17,0.977297190843239));
#23650=DIRECTION('center_axis',(-6.65798752924967E-17,1.,-1.71022579061586E-31));
#23651=DIRECTION('ref_axis',(-0.211873077029416,-1.41064830464559E-17,0.97729719084324));
#23652=DIRECTION('center_axis',(-6.65798752924967E-17,1.,-1.71022579061586E-31));
#23653=DIRECTION('ref_axis',(-0.211873077029416,-1.41064830464559E-17,0.97729719084324));
#23654=DIRECTION('center_axis',(-6.65798752924967E-17,1.,-1.71022579061586E-31));
#23655=DIRECTION('ref_axis',(-0.211873077029416,-1.41064830464559E-17,0.97729719084324));
#23656=DIRECTION('center_axis',(-6.65798752924967E-17,1.,-1.71022579061586E-31));
#23657=DIRECTION('ref_axis',(-0.211873077029416,-1.41064830464559E-17,0.97729719084324));
#23658=DIRECTION('center_axis',(-6.65798752924967E-17,1.,-1.71022579061586E-31));
#23659=DIRECTION('ref_axis',(-0.211873077029416,-1.41064830464559E-17,0.97729719084324));
#23660=DIRECTION('center_axis',(-6.65798752924967E-17,1.,-1.71022579061586E-31));
#23661=DIRECTION('ref_axis',(-0.211873077029416,-1.41064830464559E-17,0.97729719084324));
#23662=DIRECTION('center_axis',(-6.65798752924967E-17,1.,-1.71022579061586E-31));
#23663=DIRECTION('ref_axis',(-0.211873077029416,-1.41064830464559E-17,0.97729719084324));
#23664=DIRECTION('center_axis',(-6.65798752924967E-17,1.,-1.71022579061586E-31));
#23665=DIRECTION('ref_axis',(-0.211873077029416,-1.41064830464559E-17,0.97729719084324));
#23666=DIRECTION('center_axis',(-6.65798752924967E-17,1.,-1.71022579061586E-31));
#23667=DIRECTION('ref_axis',(-0.211873077029416,-1.41064830464559E-17,0.97729719084324));
#23668=DIRECTION('center_axis',(-6.65798752924967E-17,1.,-1.71022579061586E-31));
#23669=DIRECTION('ref_axis',(-0.211873077029416,-1.41064830464559E-17,0.97729719084324));
#23670=DIRECTION('center_axis',(-6.65798752924967E-17,1.,-1.71022579061586E-31));
#23671=DIRECTION('ref_axis',(-0.211873077029416,-1.41064830464559E-17,0.97729719084324));
#23672=DIRECTION('center_axis',(-6.65798752924967E-17,1.,-1.71022579061586E-31));
#23673=DIRECTION('ref_axis',(-0.211873077029416,-1.41064830464559E-17,0.97729719084324));
#23674=DIRECTION('center_axis',(-6.65798752924967E-17,1.,-1.71022579061586E-31));
#23675=DIRECTION('ref_axis',(-0.211873077029416,-1.41064830464559E-17,0.97729719084324));
#23676=DIRECTION('center_axis',(-6.65798752924967E-17,1.,-1.71022579061586E-31));
#23677=DIRECTION('ref_axis',(-0.211873077029416,-1.41064830464559E-17,0.97729719084324));
#23678=DIRECTION('center_axis',(-6.65798752924967E-17,1.,-1.71022579061586E-31));
#23679=DIRECTION('ref_axis',(-0.211873077029416,-1.41064830464559E-17,0.97729719084324));
#23680=DIRECTION('center_axis',(-6.65798752924967E-17,1.,-1.71022579061586E-31));
#23681=DIRECTION('ref_axis',(-0.211873077029416,-1.41064830464559E-17,0.97729719084324));
#23682=DIRECTION('center_axis',(-6.65798752924967E-17,1.,-1.71022579061586E-31));
#23683=DIRECTION('ref_axis',(-0.211873077029416,-1.41064830464559E-17,0.97729719084324));
#23684=DIRECTION('center_axis',(-6.65798752924967E-17,1.,-1.71022579061586E-31));
#23685=DIRECTION('ref_axis',(-0.211873077029416,-1.41064830464559E-17,0.97729719084324));
#23686=DIRECTION('center_axis',(-6.65798752924967E-17,1.,-1.71022579061586E-31));
#23687=DIRECTION('ref_axis',(-0.211873077029416,-1.41064830464559E-17,0.97729719084324));
#23688=DIRECTION('center_axis',(-6.65798752924967E-17,1.,-1.71022579061586E-31));
#23689=DIRECTION('ref_axis',(-0.211873077029416,-1.41064830464559E-17,0.97729719084324));
#23690=DIRECTION('center_axis',(-6.65798752924967E-17,1.,-1.71022579061586E-31));
#23691=DIRECTION('ref_axis',(-0.211873077029416,-1.41064830464559E-17,0.97729719084324));
#23692=DIRECTION('center_axis',(-6.65798752924967E-17,1.,-1.71022579061586E-31));
#23693=DIRECTION('ref_axis',(-0.211873077029416,-1.41064830464559E-17,0.97729719084324));
#23694=DIRECTION('center_axis',(-6.65798752924967E-17,1.,-1.71022579061586E-31));
#23695=DIRECTION('ref_axis',(-0.211873077029416,-1.41064830464559E-17,0.97729719084324));
#23696=DIRECTION('center_axis',(-6.65798752924967E-17,1.,-1.71022579061586E-31));
#23697=DIRECTION('ref_axis',(-0.211873077029416,-1.41064830464559E-17,0.97729719084324));
#23698=DIRECTION('center_axis',(-6.65798752924967E-17,1.,-1.71022579061586E-31));
#23699=DIRECTION('ref_axis',(-0.211873077029416,-1.41064830464559E-17,0.97729719084324));
#23700=DIRECTION('center_axis',(-6.65798752924967E-17,1.,-1.71022579061586E-31));
#23701=DIRECTION('ref_axis',(-0.211873077029416,-1.41064830464559E-17,0.97729719084324));
#23702=DIRECTION('center_axis',(-6.65798752924967E-17,1.,-1.71022579061586E-31));
#23703=DIRECTION('ref_axis',(-0.211873077029416,-1.41064830464559E-17,0.97729719084324));
#23704=DIRECTION('center_axis',(-6.65798752924967E-17,1.,-1.71022579061586E-31));
#23705=DIRECTION('ref_axis',(-0.211873077029416,-1.41064830464559E-17,0.97729719084324));
#23706=DIRECTION('center_axis',(-6.65798752924967E-17,1.,-1.71022579061586E-31));
#23707=DIRECTION('ref_axis',(-0.211873077029416,-1.41064830464559E-17,0.97729719084324));
#23708=DIRECTION('center_axis',(-6.65798752924967E-17,1.,-1.71022579061586E-31));
#23709=DIRECTION('ref_axis',(-0.211873077029416,-1.41064830464559E-17,0.97729719084324));
#23710=DIRECTION('center_axis',(-6.65798752924967E-17,1.,-1.71022579061586E-31));
#23711=DIRECTION('ref_axis',(-0.211873077029416,-1.41064830464559E-17,0.97729719084324));
#23712=DIRECTION('center_axis',(-6.65798752924967E-17,1.,-1.71022579061586E-31));
#23713=DIRECTION('ref_axis',(-0.211873077029416,-1.41064830464559E-17,0.97729719084324));
#23714=DIRECTION('center_axis',(-6.65798752924967E-17,1.,-1.71022579061586E-31));
#23715=DIRECTION('ref_axis',(-0.211873077029416,-1.41064830464559E-17,0.97729719084324));
#23716=DIRECTION('center_axis',(-6.65798752924967E-17,1.,-1.71022579061586E-31));
#23717=DIRECTION('ref_axis',(-0.211873077029416,-1.41064830464559E-17,0.97729719084324));
#23718=DIRECTION('center_axis',(-6.65798752924967E-17,1.,-1.71022579061586E-31));
#23719=DIRECTION('ref_axis',(-0.211873077029416,-1.41064830464559E-17,0.97729719084324));
#23720=DIRECTION('center_axis',(-6.65798752924967E-17,1.,-1.71022579061586E-31));
#23721=DIRECTION('ref_axis',(-0.211873077029416,-1.41064830464559E-17,0.97729719084324));
#23722=DIRECTION('center_axis',(-6.65798752924967E-17,1.,-1.71022579061586E-31));
#23723=DIRECTION('ref_axis',(-0.211873077029416,-1.41064830464559E-17,0.97729719084324));
#23724=DIRECTION('center_axis',(-6.65798752924967E-17,1.,-1.71022579061586E-31));
#23725=DIRECTION('ref_axis',(-0.211873077029416,-1.41064830464559E-17,0.97729719084324));
#23726=DIRECTION('center_axis',(-6.65798752924967E-17,1.,-1.71022579061586E-31));
#23727=DIRECTION('ref_axis',(-0.211873077029416,-1.41064830464559E-17,0.97729719084324));
#23728=DIRECTION('center_axis',(-6.65798752924967E-17,1.,-1.71022579061586E-31));
#23729=DIRECTION('ref_axis',(-0.211873077029416,-1.41064830464559E-17,0.97729719084324));
#23730=DIRECTION('center_axis',(-6.65798752924967E-17,1.,-1.71022579061586E-31));
#23731=DIRECTION('ref_axis',(-0.211873077029416,-1.41064830464559E-17,0.97729719084324));
#23732=DIRECTION('center_axis',(-6.65798752924967E-17,1.,-1.71022579061586E-31));
#23733=DIRECTION('ref_axis',(-0.211873077029416,-1.41064830464559E-17,0.97729719084324));
#23734=DIRECTION('center_axis',(-6.65798752924967E-17,1.,-1.71022579061586E-31));
#23735=DIRECTION('ref_axis',(-0.211873077029416,-1.41064830464559E-17,0.97729719084324));
#23736=DIRECTION('center_axis',(-6.65798752924967E-17,1.,-1.71022579061586E-31));
#23737=DIRECTION('ref_axis',(-0.211873077029416,-1.41064830464559E-17,0.97729719084324));
#23738=DIRECTION('center_axis',(6.65798752924967E-17,-1.,1.71022579061586E-31));
#23739=DIRECTION('ref_axis',(0.211873077029416,1.41064830464559E-17,-0.977297190843239));
#23740=DIRECTION('center_axis',(-6.65798752924967E-17,1.,-1.71022579061586E-31));
#23741=DIRECTION('ref_axis',(-0.211873077029416,-1.41064830464559E-17,0.977297190843239));
#23742=DIRECTION('center_axis',(6.65798752924967E-17,-1.,1.71022579061586E-31));
#23743=DIRECTION('ref_axis',(-0.211873077029416,-1.41064830464559E-17,0.97729719084324));
#23744=DIRECTION('',(-6.65798752924967E-17,1.,-1.71022579061586E-31));
#23745=DIRECTION('center_axis',(-6.65798752924967E-17,1.,-1.71022579061586E-31));
#23746=DIRECTION('ref_axis',(-0.211873077029416,-1.41064830464559E-17,0.977297190843239));
#23747=DIRECTION('',(6.65798752924967E-17,-1.,1.71022579061586E-31));
#23748=DIRECTION('center_axis',(6.65798752924967E-17,-1.,1.71022579061586E-31));
#23749=DIRECTION('ref_axis',(-0.211873077029416,-1.41064830464559E-17,0.97729719084324));
#23750=DIRECTION('center_axis',(-6.65798752924967E-17,1.,-1.71022579061586E-31));
#23751=DIRECTION('ref_axis',(-0.211873077029416,-1.41064830464559E-17,0.977297190843239));
#23752=DIRECTION('center_axis',(6.65798752924967E-17,-1.,1.71022579061586E-31));
#23753=DIRECTION('ref_axis',(-0.211873077029416,-1.41064830464559E-17,0.97729719084324));
#23754=DIRECTION('center_axis',(-6.65798752924967E-17,1.,-1.71022579061586E-31));
#23755=DIRECTION('ref_axis',(-0.211873077029416,-1.41064830464559E-17,0.977297190843239));
#23756=DIRECTION('center_axis',(6.65798752924967E-17,-1.,1.71022579061586E-31));
#23757=DIRECTION('ref_axis',(-0.211873077029416,-1.41064830464559E-17,0.97729719084324));
#23758=DIRECTION('center_axis',(-6.65798752924967E-17,1.,-1.71022579061586E-31));
#23759=DIRECTION('ref_axis',(-0.211873077029416,-1.41064830464559E-17,0.977297190843239));
#23760=DIRECTION('center_axis',(6.65798752924967E-17,-1.,1.71022579061586E-31));
#23761=DIRECTION('ref_axis',(-0.211873077029416,-1.41064830464559E-17,0.97729719084324));
#23762=DIRECTION('center_axis',(-6.65798752924967E-17,1.,-1.71022579061586E-31));
#23763=DIRECTION('ref_axis',(-0.211873077029416,-1.41064830464559E-17,0.977297190843239));
#23764=DIRECTION('center_axis',(6.65798752924967E-17,-1.,1.71022579061586E-31));
#23765=DIRECTION('ref_axis',(-0.211873077029416,-1.41064830464559E-17,0.97729719084324));
#23766=DIRECTION('center_axis',(-6.65798752924967E-17,1.,-1.71022579061586E-31));
#23767=DIRECTION('ref_axis',(-0.211873077029416,-1.41064830464559E-17,0.977297190843239));
#23768=DIRECTION('center_axis',(6.65798752924967E-17,-1.,1.71022579061586E-31));
#23769=DIRECTION('ref_axis',(-0.211873077029416,-1.41064830464559E-17,0.97729719084324));
#23770=DIRECTION('center_axis',(-6.65798752924967E-17,1.,-1.71022579061586E-31));
#23771=DIRECTION('ref_axis',(-0.211873077029416,-1.41064830464559E-17,0.977297190843239));
#23772=DIRECTION('center_axis',(6.65798752924967E-17,-1.,1.71022579061586E-31));
#23773=DIRECTION('ref_axis',(-0.211873077029416,-1.41064830464559E-17,0.97729719084324));
#23774=DIRECTION('center_axis',(-6.65798752924967E-17,1.,-1.71022579061586E-31));
#23775=DIRECTION('ref_axis',(-0.211873077029416,-1.41064830464559E-17,0.977297190843239));
#23776=DIRECTION('center_axis',(6.65798752924967E-17,-1.,1.71022579061586E-31));
#23777=DIRECTION('ref_axis',(-0.211873077029416,-1.41064830464559E-17,0.97729719084324));
#23778=DIRECTION('center_axis',(-6.65798752924967E-17,1.,-1.71022579061586E-31));
#23779=DIRECTION('ref_axis',(-0.211873077029416,-1.41064830464559E-17,0.977297190843239));
#23780=DIRECTION('center_axis',(6.65798752924967E-17,-1.,1.71022579061586E-31));
#23781=DIRECTION('ref_axis',(-0.211873077029416,-1.41064830464559E-17,0.97729719084324));
#23782=DIRECTION('center_axis',(-6.65798752924967E-17,1.,-1.71022579061586E-31));
#23783=DIRECTION('ref_axis',(-0.211873077029416,-1.41064830464559E-17,0.977297190843239));
#23784=DIRECTION('center_axis',(6.65798752924967E-17,-1.,1.71022579061586E-31));
#23785=DIRECTION('ref_axis',(-0.211873077029416,-1.41064830464559E-17,0.97729719084324));
#23786=DIRECTION('center_axis',(-6.65798752924967E-17,1.,-1.71022579061586E-31));
#23787=DIRECTION('ref_axis',(-0.211873077029416,-1.41064830464559E-17,0.977297190843239));
#23788=DIRECTION('center_axis',(6.65798752924967E-17,-1.,1.71022579061586E-31));
#23789=DIRECTION('ref_axis',(-0.211873077029416,-1.41064830464559E-17,0.97729719084324));
#23790=DIRECTION('center_axis',(-6.65798752924967E-17,1.,-1.71022579061586E-31));
#23791=DIRECTION('ref_axis',(-0.211873077029416,-1.41064830464559E-17,0.977297190843239));
#23792=DIRECTION('center_axis',(6.65798752924967E-17,-1.,1.71022579061586E-31));
#23793=DIRECTION('ref_axis',(-0.211873077029416,-1.41064830464559E-17,0.97729719084324));
#23794=DIRECTION('center_axis',(-6.65798752924967E-17,1.,-1.71022579061586E-31));
#23795=DIRECTION('ref_axis',(-0.211873077029416,-1.41064830464559E-17,0.977297190843239));
#23796=DIRECTION('center_axis',(6.65798752924967E-17,-1.,1.71022579061586E-31));
#23797=DIRECTION('ref_axis',(-0.211873077029416,-1.41064830464559E-17,0.97729719084324));
#23798=DIRECTION('center_axis',(-6.65798752924967E-17,1.,-1.71022579061586E-31));
#23799=DIRECTION('ref_axis',(-0.211873077029416,-1.41064830464559E-17,0.977297190843239));
#23800=DIRECTION('center_axis',(6.65798752924967E-17,-1.,1.71022579061586E-31));
#23801=DIRECTION('ref_axis',(-0.211873077029416,-1.41064830464559E-17,0.97729719084324));
#23802=DIRECTION('center_axis',(-6.65798752924967E-17,1.,-1.71022579061586E-31));
#23803=DIRECTION('ref_axis',(-0.211873077029416,-1.41064830464559E-17,0.977297190843239));
#23804=DIRECTION('center_axis',(6.65798752924967E-17,-1.,1.71022579061586E-31));
#23805=DIRECTION('ref_axis',(-0.211873077029416,-1.41064830464559E-17,0.97729719084324));
#23806=DIRECTION('center_axis',(-6.65798752924967E-17,1.,-1.71022579061586E-31));
#23807=DIRECTION('ref_axis',(-0.211873077029416,-1.41064830464559E-17,0.977297190843239));
#23808=DIRECTION('center_axis',(6.65798752924967E-17,-1.,1.71022579061586E-31));
#23809=DIRECTION('ref_axis',(-0.211873077029416,-1.41064830464559E-17,0.97729719084324));
#23810=DIRECTION('center_axis',(-6.65798752924967E-17,1.,-1.71022579061586E-31));
#23811=DIRECTION('ref_axis',(-0.211873077029416,-1.41064830464559E-17,0.977297190843239));
#23812=DIRECTION('center_axis',(6.65798752924967E-17,-1.,1.71022579061586E-31));
#23813=DIRECTION('ref_axis',(-0.211873077029416,-1.41064830464559E-17,0.97729719084324));
#23814=DIRECTION('center_axis',(-6.65798752924967E-17,1.,-1.71022579061586E-31));
#23815=DIRECTION('ref_axis',(-0.211873077029416,-1.41064830464559E-17,0.977297190843239));
#23816=DIRECTION('center_axis',(6.65798752924967E-17,-1.,1.71022579061586E-31));
#23817=DIRECTION('ref_axis',(-0.211873077029416,-1.41064830464559E-17,0.97729719084324));
#23818=DIRECTION('center_axis',(-6.65798752924967E-17,1.,-1.71022579061586E-31));
#23819=DIRECTION('ref_axis',(-0.211873077029416,-1.41064830464559E-17,0.977297190843239));
#23820=DIRECTION('center_axis',(6.65798752924967E-17,-1.,1.71022579061586E-31));
#23821=DIRECTION('ref_axis',(-0.211873077029416,-1.41064830464559E-17,0.97729719084324));
#23822=DIRECTION('center_axis',(-6.65798752924967E-17,1.,-1.71022579061586E-31));
#23823=DIRECTION('ref_axis',(-0.211873077029416,-1.41064830464559E-17,0.977297190843239));
#23824=DIRECTION('center_axis',(6.65798752924967E-17,-1.,1.71022579061586E-31));
#23825=DIRECTION('ref_axis',(-0.211873077029416,-1.41064830464559E-17,0.97729719084324));
#23826=DIRECTION('center_axis',(-6.65798752924967E-17,1.,-1.71022579061586E-31));
#23827=DIRECTION('ref_axis',(-0.211873077029416,-1.41064830464559E-17,0.977297190843239));
#23828=DIRECTION('center_axis',(6.65798752924967E-17,-1.,1.71022579061586E-31));
#23829=DIRECTION('ref_axis',(-0.211873077029416,-1.41064830464559E-17,0.97729719084324));
#23830=DIRECTION('center_axis',(-6.65798752924967E-17,1.,-1.71022579061586E-31));
#23831=DIRECTION('ref_axis',(-0.211873077029416,-1.41064830464559E-17,0.977297190843239));
#23832=DIRECTION('center_axis',(6.65798752924967E-17,-1.,1.71022579061586E-31));
#23833=DIRECTION('ref_axis',(-0.211873077029416,-1.41064830464559E-17,0.97729719084324));
#23834=DIRECTION('center_axis',(-6.65798752924967E-17,1.,-1.71022579061586E-31));
#23835=DIRECTION('ref_axis',(-0.211873077029416,-1.41064830464559E-17,0.977297190843239));
#23836=DIRECTION('center_axis',(6.65798752924967E-17,-1.,1.71022579061586E-31));
#23837=DIRECTION('ref_axis',(-0.211873077029416,-1.41064830464559E-17,0.97729719084324));
#23838=DIRECTION('center_axis',(-6.65798752924967E-17,1.,-1.71022579061586E-31));
#23839=DIRECTION('ref_axis',(-0.211873077029416,-1.41064830464559E-17,0.977297190843239));
#23840=DIRECTION('center_axis',(6.65798752924967E-17,-1.,1.71022579061586E-31));
#23841=DIRECTION('ref_axis',(-0.211873077029416,-1.41064830464559E-17,0.97729719084324));
#23842=DIRECTION('center_axis',(-6.65798752924967E-17,1.,-1.71022579061586E-31));
#23843=DIRECTION('ref_axis',(-0.211873077029416,-1.41064830464559E-17,0.977297190843239));
#23844=DIRECTION('center_axis',(6.65798752924967E-17,-1.,1.71022579061586E-31));
#23845=DIRECTION('ref_axis',(-0.211873077029416,-1.41064830464559E-17,0.97729719084324));
#23846=DIRECTION('center_axis',(-6.65798752924967E-17,1.,-1.71022579061586E-31));
#23847=DIRECTION('ref_axis',(-0.211873077029416,-1.41064830464559E-17,0.977297190843239));
#23848=DIRECTION('center_axis',(6.65798752924967E-17,-1.,1.71022579061586E-31));
#23849=DIRECTION('ref_axis',(-0.211873077029416,-1.41064830464559E-17,0.97729719084324));
#23850=DIRECTION('center_axis',(-6.65798752924967E-17,1.,-1.71022579061586E-31));
#23851=DIRECTION('ref_axis',(-0.211873077029416,-1.41064830464559E-17,0.977297190843239));
#23852=DIRECTION('center_axis',(6.65798752924967E-17,-1.,1.71022579061586E-31));
#23853=DIRECTION('ref_axis',(-0.211873077029416,-1.41064830464559E-17,0.97729719084324));
#23854=DIRECTION('center_axis',(-6.65798752924967E-17,1.,-1.71022579061586E-31));
#23855=DIRECTION('ref_axis',(-0.211873077029416,-1.41064830464559E-17,0.977297190843239));
#23856=DIRECTION('center_axis',(6.65798752924967E-17,-1.,1.71022579061586E-31));
#23857=DIRECTION('ref_axis',(-0.211873077029416,-1.41064830464559E-17,0.97729719084324));
#23858=DIRECTION('center_axis',(-6.65798752924967E-17,1.,-1.71022579061586E-31));
#23859=DIRECTION('ref_axis',(-0.211873077029416,-1.41064830464559E-17,0.977297190843239));
#23860=DIRECTION('center_axis',(6.65798752924967E-17,-1.,1.71022579061586E-31));
#23861=DIRECTION('ref_axis',(-0.211873077029416,-1.41064830464559E-17,0.97729719084324));
#23862=DIRECTION('center_axis',(-6.65798752924967E-17,1.,-1.71022579061586E-31));
#23863=DIRECTION('ref_axis',(-0.211873077029416,-1.41064830464559E-17,0.977297190843239));
#23864=DIRECTION('center_axis',(6.65798752924967E-17,-1.,1.71022579061586E-31));
#23865=DIRECTION('ref_axis',(-0.211873077029416,-1.41064830464559E-17,0.97729719084324));
#23866=DIRECTION('center_axis',(-6.65798752924967E-17,1.,-1.71022579061586E-31));
#23867=DIRECTION('ref_axis',(-0.211873077029416,-1.41064830464559E-17,0.977297190843239));
#23868=DIRECTION('center_axis',(6.65798752924967E-17,-1.,1.71022579061586E-31));
#23869=DIRECTION('ref_axis',(-0.211873077029416,-1.41064830464559E-17,0.97729719084324));
#23870=DIRECTION('center_axis',(-6.65798752924967E-17,1.,-1.71022579061586E-31));
#23871=DIRECTION('ref_axis',(-0.211873077029416,-1.41064830464559E-17,0.977297190843239));
#23872=DIRECTION('center_axis',(6.65798752924967E-17,-1.,1.71022579061586E-31));
#23873=DIRECTION('ref_axis',(-0.211873077029416,-1.41064830464559E-17,0.97729719084324));
#23874=DIRECTION('center_axis',(-6.65798752924967E-17,1.,-1.71022579061586E-31));
#23875=DIRECTION('ref_axis',(-0.211873077029416,-1.41064830464559E-17,0.977297190843239));
#23876=DIRECTION('center_axis',(6.65798752924967E-17,-1.,1.71022579061586E-31));
#23877=DIRECTION('ref_axis',(-0.211873077029416,-1.41064830464559E-17,0.97729719084324));
#23878=DIRECTION('center_axis',(-6.65798752924967E-17,1.,-1.71022579061586E-31));
#23879=DIRECTION('ref_axis',(-0.211873077029416,-1.41064830464559E-17,0.977297190843239));
#23880=DIRECTION('center_axis',(6.65798752924967E-17,-1.,1.71022579061586E-31));
#23881=DIRECTION('ref_axis',(-0.211873077029416,-1.41064830464559E-17,0.97729719084324));
#23882=DIRECTION('center_axis',(-6.65798752924967E-17,1.,-1.71022579061586E-31));
#23883=DIRECTION('ref_axis',(-0.211873077029416,-1.41064830464559E-17,0.977297190843239));
#23884=DIRECTION('center_axis',(6.65798752924967E-17,-1.,1.71022579061586E-31));
#23885=DIRECTION('ref_axis',(-0.211873077029416,-1.41064830464559E-17,0.97729719084324));
#23886=DIRECTION('center_axis',(-6.65798752924967E-17,1.,-1.71022579061586E-31));
#23887=DIRECTION('ref_axis',(-0.211873077029416,-1.41064830464559E-17,0.977297190843239));
#23888=DIRECTION('center_axis',(6.65798752924967E-17,-1.,1.71022579061586E-31));
#23889=DIRECTION('ref_axis',(-0.211873077029416,-1.41064830464559E-17,0.97729719084324));
#23890=DIRECTION('center_axis',(-6.65798752924967E-17,1.,-1.71022579061586E-31));
#23891=DIRECTION('ref_axis',(-0.211873077029416,-1.41064830464559E-17,0.977297190843239));
#23892=DIRECTION('center_axis',(6.65798752924967E-17,-1.,1.71022579061586E-31));
#23893=DIRECTION('ref_axis',(-0.211873077029416,-1.41064830464559E-17,0.97729719084324));
#23894=DIRECTION('center_axis',(-6.65798752924967E-17,1.,-1.71022579061586E-31));
#23895=DIRECTION('ref_axis',(-0.211873077029416,-1.41064830464559E-17,0.977297190843239));
#23896=DIRECTION('center_axis',(6.65798752924967E-17,-1.,1.71022579061586E-31));
#23897=DIRECTION('ref_axis',(-0.211873077029416,-1.41064830464559E-17,0.97729719084324));
#23898=DIRECTION('center_axis',(-6.65798752924967E-17,1.,-1.71022579061586E-31));
#23899=DIRECTION('ref_axis',(-0.211873077029416,-1.41064830464559E-17,0.977297190843239));
#23900=DIRECTION('center_axis',(6.65798752924967E-17,-1.,1.71022579061586E-31));
#23901=DIRECTION('ref_axis',(-0.211873077029416,-1.41064830464559E-17,0.97729719084324));
#23902=DIRECTION('center_axis',(-6.65798752924967E-17,1.,-1.71022579061586E-31));
#23903=DIRECTION('ref_axis',(-0.211873077029416,-1.41064830464559E-17,0.977297190843239));
#23904=DIRECTION('center_axis',(6.65798752924967E-17,-1.,1.71022579061586E-31));
#23905=DIRECTION('ref_axis',(-0.211873077029416,-1.41064830464559E-17,0.97729719084324));
#23906=DIRECTION('center_axis',(-6.65798752924967E-17,1.,-1.71022579061586E-31));
#23907=DIRECTION('ref_axis',(-0.211873077029416,-1.41064830464559E-17,0.977297190843239));
#23908=DIRECTION('center_axis',(6.65798752924967E-17,-1.,1.71022579061586E-31));
#23909=DIRECTION('ref_axis',(-0.211873077029416,-1.41064830464559E-17,0.97729719084324));
#23910=DIRECTION('center_axis',(-6.65798752924967E-17,1.,-1.71022579061586E-31));
#23911=DIRECTION('ref_axis',(-0.211873077029416,-1.41064830464559E-17,0.977297190843239));
#23912=DIRECTION('center_axis',(6.65798752924967E-17,-1.,1.71022579061586E-31));
#23913=DIRECTION('ref_axis',(-0.211873077029416,-1.41064830464559E-17,0.97729719084324));
#23914=DIRECTION('center_axis',(-6.65798752924967E-17,1.,-1.71022579061586E-31));
#23915=DIRECTION('ref_axis',(-0.211873077029416,-1.41064830464559E-17,0.977297190843239));
#23916=DIRECTION('center_axis',(6.65798752924967E-17,-1.,1.71022579061586E-31));
#23917=DIRECTION('ref_axis',(-0.211873077029416,-1.41064830464559E-17,0.97729719084324));
#23918=DIRECTION('center_axis',(6.65798752924967E-17,-1.,1.71022579061586E-31));
#23919=DIRECTION('ref_axis',(-0.211873077029416,-1.41064830464559E-17,0.977297190843239));
#23920=DIRECTION('center_axis',(-6.65798752924967E-17,1.,-1.71022579061586E-31));
#23921=DIRECTION('ref_axis',(-0.211873077029416,-1.41064830464559E-17,0.977297190843239));
#23922=DIRECTION('center_axis',(6.65798752924967E-17,-1.,1.71022579061586E-31));
#23923=DIRECTION('ref_axis',(0.97729719084324,6.50683250900503E-17,0.211873077029416));
#23924=DIRECTION('center_axis',(6.65798752924967E-17,-1.,1.71022579061586E-31));
#23925=DIRECTION('ref_axis',(-0.211873077029416,-1.41064830464559E-17,0.97729719084324));
#23926=DIRECTION('center_axis',(-6.65798752924967E-17,1.,-1.71022579061586E-31));
#23927=DIRECTION('ref_axis',(0.211873077029416,1.41064830464559E-17,-0.977297190843239));
#23928=DIRECTION('center_axis',(-6.65798752924967E-17,1.,-1.71022579061586E-31));
#23929=DIRECTION('ref_axis',(-0.211873077029416,-1.41064830464559E-17,0.977297190843239));
#23930=DIRECTION('center_axis',(-6.65798752924967E-17,1.,-1.71022579061586E-31));
#23931=DIRECTION('ref_axis',(0.211873077029416,1.41064830464559E-17,-0.97729719084324));
#23932=DIRECTION('',(-6.65798752924967E-17,1.,-1.71022579061586E-31));
#23933=DIRECTION('axis',(0.,0.,1.));
#23934=DIRECTION('refdir',(1.,0.,0.));
#23935=DIRECTION('center_axis',(-4.64905891561784E-16,0.,-1.));
#23936=DIRECTION('ref_axis',(1.,2.80259692864963E-45,-4.64905891561784E-16));
#23937=DIRECTION('',(-1.,1.13620248180482E-13,4.64905891561784E-16));
#23938=DIRECTION('',(0.,-1.,0.));
#23939=DIRECTION('',(1.,6.02124417213198E-17,-4.64905891561784E-16));
#23940=DIRECTION('',(0.,-1.,0.));
#23941=DIRECTION('center_axis',(0.,-1.,0.));
#23942=DIRECTION('ref_axis',(5.06308189820828E-12,0.,1.));
#23943=DIRECTION('center_axis',(-1.51811166660813E-15,-0.0174524064372836,
0.999847695156391));
#23944=DIRECTION('ref_axis',(8.83629631127843E-14,0.999847695156391,0.0174524064372836));
#23945=DIRECTION('center_axis',(-6.02124417213198E-17,1.,-2.60927675461843E-32));
#23946=DIRECTION('ref_axis',(5.06308189820828E-12,0.,1.));
#23947=DIRECTION('',(0.,-1.,0.));
#23948=DIRECTION('center_axis',(-1.02201073032319E-15,-0.713250449154181,
0.700909264299851));
#23949=DIRECTION('ref_axis',(3.61124543800146E-12,0.700909264299851,0.713250449154181));
#23950=DIRECTION('center_axis',(0.,-1.,0.));
#23951=DIRECTION('ref_axis',(-0.560568426943144,0.,0.828108108108168));
#23952=DIRECTION('center_axis',(-1.02201073032319E-15,-0.713250449154181,
0.700909264299851));
#23953=DIRECTION('ref_axis',(-1.0085471152714E-15,0.700909264299851,0.713250449154181));
#23954=DIRECTION('center_axis',(-6.02124417213198E-17,1.,-2.60927675461843E-32));
#23955=DIRECTION('ref_axis',(-0.560568426943144,0.,0.828108108108168));
#23956=DIRECTION('',(0.,-1.,0.));
#23957=DIRECTION('center_axis',(-0.700909264299851,-0.713250449154181,-1.06495728142559E-15));
#23958=DIRECTION('ref_axis',(-0.713250449154181,0.700909264299851,-1.19764969938479E-15));
#23959=DIRECTION('center_axis',(6.02124417213198E-17,-1.,2.60927675461843E-32));
#23960=DIRECTION('ref_axis',(-0.560568426943144,0.,0.828108108108168));
#23961=DIRECTION('center_axis',(6.02124417213198E-17,-1.,2.60927675461843E-32));
#23962=DIRECTION('ref_axis',(-0.560568426943144,0.,0.828108108108168));
#23963=DIRECTION('center_axis',(0.,-1.,0.));
#23964=DIRECTION('ref_axis',(-0.828108108108883,0.,0.560568426942087));
#23965=DIRECTION('center_axis',(-0.700909264299851,-0.713250449154181,-1.06495728142559E-15));
#23966=DIRECTION('ref_axis',(-0.713250449154181,0.700909264299851,-1.0888172225833E-15));
#23967=DIRECTION('center_axis',(-6.02124417213198E-17,1.,-2.60927675461843E-32));
#23968=DIRECTION('ref_axis',(-0.828108108108883,0.,0.560568426942087));
#23969=DIRECTION('',(0.,-1.,0.));
#23970=DIRECTION('center_axis',(-0.999847695156391,-0.0174524064372837,
-1.51916251861363E-15));
#23971=DIRECTION('ref_axis',(-0.0174524064372837,0.999847695156391,-2.66420872597733E-17));
#23972=DIRECTION('center_axis',(1.,0.,-1.22327594243755E-16));
#23973=DIRECTION('ref_axis',(1.22327594243755E-16,5.79319727271681E-31,
1.));
#23974=DIRECTION('',(-1.22327594243755E-16,9.40541631133221E-14,-1.));
#23975=DIRECTION('',(1.22327594243755E-16,3.34584106854956E-32,1.));
#23976=DIRECTION('',(0.,-1.,0.));
#23977=DIRECTION('center_axis',(0.,-1.,0.));
#23978=DIRECTION('ref_axis',(-1.,0.,5.0097911930254E-12));
#23979=DIRECTION('center_axis',(-0.999847695156391,-0.0174524064372837,
-1.51916251861363E-15));
#23980=DIRECTION('ref_axis',(-0.0174524064372837,0.999847695156391,8.74329120666037E-14));
#23981=DIRECTION('center_axis',(-6.02124417213198E-17,1.,-2.60927675461843E-32));
#23982=DIRECTION('ref_axis',(-1.,0.,5.0097911930254E-12));
#23983=DIRECTION('',(0.,-1.,0.));
#23984=DIRECTION('center_axis',(-0.700909264299851,-0.713250449154181,-1.06495728142559E-15));
#23985=DIRECTION('ref_axis',(-0.713250449154181,0.700909264299851,3.57323581859403E-12));
#23986=DIRECTION('center_axis',(0.,-1.,0.));
#23987=DIRECTION('ref_axis',(-0.828108108107798,0.,-0.56056842694369));
#23988=DIRECTION('center_axis',(-0.700909264299851,-0.713250449154181,-1.06495728142559E-15));
#23989=DIRECTION('ref_axis',(-0.713250449154181,0.700909264299851,-1.19764969938473E-15));
#23990=DIRECTION('center_axis',(-6.02124417213198E-17,1.,-2.60927675461843E-32));
#23991=DIRECTION('ref_axis',(-0.828108108107798,0.,-0.56056842694369));
#23992=DIRECTION('',(0.,-1.,0.));
#23993=DIRECTION('center_axis',(1.10790383252799E-15,-0.713250449154181,
-0.700909264299851));
#23994=DIRECTION('ref_axis',(1.19764969938473E-15,0.700909264299851,-0.713250449154181));
#23995=DIRECTION('center_axis',(6.02124417213198E-17,-1.,2.60927675461843E-32));
#23996=DIRECTION('ref_axis',(-0.828108108107798,0.,-0.56056842694369));
#23997=DIRECTION('center_axis',(6.02124417213198E-17,-1.,2.60927675461843E-32));
#23998=DIRECTION('ref_axis',(-0.828108108107798,0.,-0.56056842694369));
#23999=DIRECTION('center_axis',(0.,-1.,0.));
#24000=DIRECTION('ref_axis',(-0.560568426942121,0.,-0.82810810810886));
#24001=DIRECTION('center_axis',(1.10790383252799E-15,-0.713250449154181,
-0.700909264299851));
#24002=DIRECTION('ref_axis',(1.0888172225922E-15,0.700909264299851,-0.713250449154181));
#24003=DIRECTION('center_axis',(-6.02124417213198E-17,1.,-2.60927675461843E-32));
#24004=DIRECTION('ref_axis',(-0.560568426942121,0.,-0.82810810810886));
#24005=DIRECTION('',(0.,-1.,0.));
#24006=DIRECTION('center_axis',(1.52021337061914E-15,-0.0174524064372836,
-0.999847695156391));
#24007=DIRECTION('ref_axis',(2.66420872599909E-17,0.999847695156391,-0.0174524064372836));
#24008=DIRECTION('center_axis',(8.71984094268636E-13,0.,1.));
#24009=DIRECTION('ref_axis',(-1.,-2.54388977262688E-34,8.71984094268636E-13));
#24010=DIRECTION('',(1.,5.00430415356568E-11,-8.71984094268635E-13));
#24011=DIRECTION('',(-1.,-6.02124417213198E-17,8.71984094268636E-13));
#24012=DIRECTION('',(0.,-1.,0.));
#24013=DIRECTION('center_axis',(0.,-1.,0.));
#24014=DIRECTION('ref_axis',(-4.92541424309684E-12,0.,-1.));
#24015=DIRECTION('center_axis',(1.52021337061914E-15,-0.0174524064372836,
-0.999847695156391));
#24016=DIRECTION('ref_axis',(-8.59603312425117E-14,0.999847695156391,-0.0174524064372836));
#24017=DIRECTION('center_axis',(-6.02124417213198E-17,1.,-2.60927675461843E-32));
#24018=DIRECTION('ref_axis',(-4.92541424309684E-12,0.,-1.));
#24019=DIRECTION('',(0.,-1.,0.));
#24020=DIRECTION('center_axis',(1.10790383252799E-15,-0.713250449154181,
-0.700909264299851));
#24021=DIRECTION('ref_axis',(-3.51305392115922E-12,0.700909264299851,-0.713250449154181));
#24022=DIRECTION('center_axis',(0.,-1.,0.));
#24023=DIRECTION('ref_axis',(0.560568426943322,0.,-0.828108108108047));
#24024=DIRECTION('center_axis',(1.10790383252799E-15,-0.713250449154181,
-0.700909264299851));
#24025=DIRECTION('ref_axis',(1.13461550468027E-15,0.700909264299851,-0.713250449154181));
#24026=DIRECTION('center_axis',(-6.02124417213198E-17,1.,-2.60927675461843E-32));
#24027=DIRECTION('ref_axis',(0.560568426943322,0.,-0.828108108108047));
#24028=DIRECTION('',(0.,-1.,0.));
#24029=DIRECTION('center_axis',(0.700909264299845,-0.713250449154187,1.06495728142558E-15));
#24030=DIRECTION('ref_axis',(0.713250449154187,0.700909264299845,1.00854711527136E-15));
#24031=DIRECTION('center_axis',(6.02124417213198E-17,-1.,2.60927675461843E-32));
#24032=DIRECTION('ref_axis',(0.560568426943322,0.,-0.828108108108047));
#24033=DIRECTION('center_axis',(6.02124417213198E-17,-1.,2.60927675461843E-32));
#24034=DIRECTION('ref_axis',(0.560568426943322,0.,-0.828108108108047));
#24035=DIRECTION('center_axis',(-1.,0.,-8.67628499512335E-13));
#24036=DIRECTION('ref_axis',(8.67628499512335E-13,-5.79319727271681E-31,
-1.));
#24037=DIRECTION('',(8.67628499512335E-13,5.22159376950964E-29,-1.));
#24038=DIRECTION('',(0.,-1.,0.));
#24039=DIRECTION('',(-6.13505995555881E-13,-0.707106781186547,0.707106781186548));
#24040=DIRECTION('',(5.67373952042745E-44,-1.,-6.53936508957056E-32));
#24041=DIRECTION('center_axis',(-1.,0.,-8.67628499512335E-13));
#24042=DIRECTION('ref_axis',(8.67628499512335E-13,-5.79319727271681E-31,
-1.));
#24043=DIRECTION('',(8.67628499512335E-13,5.22159376950964E-29,-1.));
#24044=DIRECTION('',(-5.67373952042745E-44,1.,6.53936508957056E-32));
#24045=DIRECTION('',(-6.13505995555881E-13,0.707106781186547,0.707106781186548));
#24046=DIRECTION('',(0.,1.,0.));
#24047=DIRECTION('center_axis',(-4.64905891561784E-16,0.,-1.));
#24048=DIRECTION('ref_axis',(1.,2.80259692864963E-45,-4.64905891561784E-16));
#24049=DIRECTION('',(1.,6.02124417213198E-17,-4.64905891561784E-16));
#24050=DIRECTION('',(-1.,1.92408737950894E-15,4.64905891561784E-16));
#24051=DIRECTION('',(-0.707106781186548,-0.707106781186547,3.28738108536916E-16));
#24052=DIRECTION('',(6.02124417213198E-17,-1.,-2.79931189015622E-32));
#24053=DIRECTION('center_axis',(-1.,0.,-8.67628499512335E-13));
#24054=DIRECTION('ref_axis',(8.67628499512335E-13,-5.79319727271681E-31,
-1.));
#24055=DIRECTION('',(-8.67628499512335E-13,-4.96193574268823E-11,1.));
#24056=DIRECTION('',(4.61918851910391E-44,-1.,-5.32392437742675E-32));
#24057=DIRECTION('',(8.67628499512335E-13,5.22159376950964E-29,-1.));
#24058=DIRECTION('',(0.,-1.,0.));
#24059=DIRECTION('center_axis',(0.,-1.,0.));
#24060=DIRECTION('ref_axis',(1.,0.,-5.00979119302536E-12));
#24061=DIRECTION('center_axis',(0.700909264299845,-0.713250449154187,1.06495728142558E-15));
#24062=DIRECTION('ref_axis',(0.713250449154187,0.700909264299845,-3.57323581859403E-12));
#24063=DIRECTION('center_axis',(0.999847695156391,-0.0174524064372835,1.51916251861363E-15));
#24064=DIRECTION('ref_axis',(0.0174524064372835,0.999847695156391,-8.74329120666019E-14));
#24065=DIRECTION('center_axis',(-6.02124417213198E-17,1.,-2.60927675461843E-32));
#24066=DIRECTION('ref_axis',(1.,0.,-5.00979119302536E-12));
#24067=DIRECTION('',(0.,-1.,0.));
#24068=DIRECTION('center_axis',(0.,-1.,0.));
#24069=DIRECTION('ref_axis',(0.828108108108418,0.,0.560568426942775));
#24070=DIRECTION('center_axis',(-1.02201073032319E-15,-0.713250449154181,
0.700909264299851));
#24071=DIRECTION('ref_axis',(-1.07158130997516E-15,0.700909264299851,0.713250449154181));
#24072=DIRECTION('center_axis',(6.02124417213198E-17,-1.,2.60927675461843E-32));
#24073=DIRECTION('ref_axis',(0.828108108108418,0.,0.560568426942775));
#24074=DIRECTION('center_axis',(6.02124417213198E-17,-1.,2.60927675461843E-32));
#24075=DIRECTION('ref_axis',(0.828108108108418,0.,0.560568426942775));
#24076=DIRECTION('center_axis',(0.700909264299845,-0.713250449154187,1.06495728142558E-15));
#24077=DIRECTION('ref_axis',(0.713250449154187,0.700909264299845,1.19764969938401E-15));
#24078=DIRECTION('center_axis',(-6.02124417213198E-17,1.,-2.60927675461843E-32));
#24079=DIRECTION('ref_axis',(0.828108108108418,0.,0.560568426942775));
#24080=DIRECTION('',(0.,-1.,0.));
#24081=DIRECTION('center_axis',(0.,-1.,0.));
#24082=DIRECTION('ref_axis',(0.560568426942125,0.,0.828108108108858));
#24083=DIRECTION('center_axis',(-1.51811166660813E-15,-0.0174524064372836,
0.999847695156391));
#24084=DIRECTION('ref_axis',(-2.664208725992E-17,0.999847695156391,0.0174524064372836));
#24085=DIRECTION('center_axis',(-1.02201073032319E-15,-0.713250449154181,
0.700909264299851));
#24086=DIRECTION('ref_axis',(-9.89833838717548E-16,0.700909264299851,0.713250449154181));
#24087=DIRECTION('center_axis',(-6.02124417213198E-17,1.,-2.60927675461843E-32));
#24088=DIRECTION('ref_axis',(0.560568426942125,0.,0.828108108108858));
#24089=DIRECTION('center_axis',(0.,-1.,0.));
#24090=DIRECTION('ref_axis',(0.828108108108829,0.,-0.560568426942167));
#24091=DIRECTION('center_axis',(-6.02124417213198E-17,1.,-2.60927675461843E-32));
#24092=DIRECTION('ref_axis',(0.828108108108829,0.,-0.560568426942167));
#24093=DIRECTION('',(0.,-1.,0.));
#24094=DIRECTION('center_axis',(0.999847695156391,-0.0174524064372835,1.51916251861363E-15));
#24095=DIRECTION('ref_axis',(0.0174524064372835,0.999847695156391,2.42200793274045E-17));
#24096=DIRECTION('center_axis',(0.700909264299845,-0.713250449154187,1.06495728142558E-15));
#24097=DIRECTION('ref_axis',(0.713250449154187,0.700909264299845,1.1878006064711E-15));
#24098=DIRECTION('center_axis',(-1.,0.,-8.67628499512335E-13));
#24099=DIRECTION('ref_axis',(8.67628499512335E-13,-5.79319727271681E-31,
-1.));
#24100=DIRECTION('',(8.67628499512335E-13,5.22159376950964E-29,-1.));
#24101=DIRECTION('',(-2.1384182212495E-44,1.,2.46467033119755E-32));
#24102=DIRECTION('',(-8.67628499512335E-13,-4.96193574268823E-11,1.));
#24103=DIRECTION('center_axis',(4.64905891561784E-16,0.,1.));
#24104=DIRECTION('ref_axis',(-1.,-2.80259692864963E-45,4.64905891561784E-16));
#24105=DIRECTION('',(-1.,-6.02124417213198E-17,4.64905891561784E-16));
#24106=DIRECTION('',(-6.02124417213198E-17,1.,2.79931189015621E-32));
#24107=DIRECTION('',(0.707106781186546,0.70710678118655,-3.28738108536915E-16));
#24108=DIRECTION('',(1.,2.04451226295158E-15,-4.64905891561784E-16));
#24109=DIRECTION('center_axis',(-1.51811166660813E-15,-0.0174524064372836,
0.999847695156391));
#24110=DIRECTION('ref_axis',(-1.,-6.02124417213198E-17,-1.51939392966847E-15));
#24111=DIRECTION('',(-1.,-6.02124417213198E-17,-1.51939392966847E-15));
#24112=DIRECTION('center_axis',(6.02124417213198E-17,-1.,2.60927675461843E-32));
#24113=DIRECTION('ref_axis',(-1.,-6.02124417213198E-17,-1.51939392966847E-15));
#24114=DIRECTION('center_axis',(-6.02124417213198E-17,1.,-2.60927675461843E-32));
#24115=DIRECTION('ref_axis',(-1.,-6.02124417213198E-17,-1.51939392966847E-15));
#24116=DIRECTION('',(0.707106781186546,-0.707106781186548,1.1609693565858E-15));
#24117=DIRECTION('center_axis',(6.02124417213198E-17,-1.,2.60927675461843E-32));
#24118=DIRECTION('ref_axis',(-1.,-6.02124417213198E-17,-1.51939392966847E-15));
#24119=DIRECTION('center_axis',(6.02124417213198E-17,-1.,2.60927675461843E-32));
#24120=DIRECTION('ref_axis',(-1.,-6.02124417213198E-17,-1.51939392966847E-15));
#24121=DIRECTION('center_axis',(-6.02124417213198E-17,1.,-2.60927675461843E-32));
#24122=DIRECTION('ref_axis',(-1.,-6.02124417213198E-17,-1.51939392966847E-15));
#24123=DIRECTION('center_axis',(-0.999847695156391,-0.0174524064372837,
-1.51916251861363E-15));
#24124=DIRECTION('ref_axis',(1.51939392966847E-15,3.89938443409397E-32,
-1.));
#24125=DIRECTION('',(1.51939392966847E-15,6.53936508957056E-32,-1.));
#24126=DIRECTION('center_axis',(-0.700909264299851,-0.713250449154181,-1.06495728142559E-15));
#24127=DIRECTION('ref_axis',(1.51939392966847E-15,2.11007687440828E-30,
-1.));
#24128=DIRECTION('',(-1.51939392966847E-15,-6.53936508957056E-32,1.));
#24129=DIRECTION('center_axis',(6.02124417213198E-17,-1.,2.60927675461843E-32));
#24130=DIRECTION('ref_axis',(-1.,-6.02124417213198E-17,-1.51939392966847E-15));
#24131=DIRECTION('center_axis',(-6.02124417213198E-17,1.,-2.60927675461843E-32));
#24132=DIRECTION('ref_axis',(-1.,-6.02124417213198E-17,-1.51939392966847E-15));
#24133=DIRECTION('',(0.707106781186546,-0.707106781186548,1.1609693565858E-15));
#24134=DIRECTION('center_axis',(6.02124417213198E-17,-1.,2.60927675461843E-32));
#24135=DIRECTION('ref_axis',(-1.,-6.02124417213198E-17,-1.51939392966847E-15));
#24136=DIRECTION('center_axis',(6.02124417213198E-17,-1.,2.60927675461843E-32));
#24137=DIRECTION('ref_axis',(-1.,-6.02124417213198E-17,-1.51939392966847E-15));
#24138=DIRECTION('center_axis',(-6.02124417213198E-17,1.,-2.60927675461843E-32));
#24139=DIRECTION('ref_axis',(-1.,-6.02124417213198E-17,-1.51939392966847E-15));
#24140=DIRECTION('center_axis',(1.52021337061914E-15,-0.0174524064372836,
-0.999847695156391));
#24141=DIRECTION('ref_axis',(1.,6.02124417213199E-17,1.51939392966848E-15));
#24142=DIRECTION('',(1.,6.02124417213198E-17,1.51939392966847E-15));
#24143=DIRECTION('center_axis',(1.10790383252799E-15,-0.713250449154181,
-0.700909264299851));
#24144=DIRECTION('ref_axis',(1.,6.02124417213211E-17,1.51939392966847E-15));
#24145=DIRECTION('',(-1.,-6.02124417213198E-17,-1.51939392966847E-15));
#24146=DIRECTION('center_axis',(6.02124417213198E-17,-1.,2.60927675461843E-32));
#24147=DIRECTION('ref_axis',(-1.,-6.02124417213198E-17,-1.51939392966847E-15));
#24148=DIRECTION('center_axis',(-6.02124417213198E-17,1.,-2.60927675461843E-32));
#24149=DIRECTION('ref_axis',(-1.,-6.02124417213198E-17,-1.51939392966847E-15));
#24150=DIRECTION('',(0.707106781186546,-0.707106781186548,1.1609693565858E-15));
#24151=DIRECTION('center_axis',(6.02124417213198E-17,-1.,2.60927675461843E-32));
#24152=DIRECTION('ref_axis',(-1.,-6.02124417213198E-17,-1.51939392966847E-15));
#24153=DIRECTION('center_axis',(6.02124417213198E-17,-1.,2.60927675461843E-32));
#24154=DIRECTION('ref_axis',(-1.,-6.02124417213198E-17,-1.51939392966847E-15));
#24155=DIRECTION('center_axis',(-6.02124417213198E-17,1.,-2.60927675461843E-32));
#24156=DIRECTION('ref_axis',(-1.,-6.02124417213198E-17,-1.51939392966847E-15));
#24157=DIRECTION('center_axis',(0.700909264299845,-0.713250449154187,1.06495728142558E-15));
#24158=DIRECTION('ref_axis',(-1.51939392966847E-15,1.65690546530681E-30,
1.));
#24159=DIRECTION('',(1.51939392966847E-15,6.53936508957056E-32,-1.));
#24160=DIRECTION('',(0.584067929597373,0.573961955888994,-0.573961955888993));
#24161=DIRECTION('',(1.51939392966847E-15,6.53936508957056E-32,-1.));
#24162=DIRECTION('center_axis',(1.51939392966847E-15,6.53936508957056E-32,
-1.));
#24163=DIRECTION('ref_axis',(1.,6.02124417213198E-17,1.51939392966847E-15));
#24164=DIRECTION('',(1.,6.02124417213198E-17,1.51939392966847E-15));
#24165=DIRECTION('',(-0.0174524064382658,-0.999847695156374,-2.6517080400408E-17));
#24166=DIRECTION('',(1.,6.02124417213198E-17,1.51939392966847E-15));
#24167=DIRECTION('center_axis',(1.1169503768152E-15,-0.707106781186548,
-0.707106781186547));
#24168=DIRECTION('ref_axis',(1.,6.02124417213228E-17,1.51939392966847E-15));
#24169=DIRECTION('',(1.01152894254293E-12,-0.707106781186547,0.707106781186548));
#24170=DIRECTION('',(-1.,-6.02124417213198E-17,-1.51939392966847E-15));
#24171=DIRECTION('',(0.0123416547519202,0.707052927141238,-0.707052927141238));
#24172=DIRECTION('center_axis',(0.707106781186547,4.2576625852945E-17,0.707106781186549));
#24173=DIRECTION('ref_axis',(-6.02124417213198E-17,1.,-9.64348767934759E-33));
#24174=DIRECTION('',(0.707106781186548,4.25766258529451E-17,-0.707106781186547));
#24175=DIRECTION('',(-6.02124417213198E-17,1.,-2.60927675461843E-32));
#24176=DIRECTION('',(-0.707106781186548,-4.25766258529451E-17,0.707106781186547));
#24177=DIRECTION('center_axis',(6.02124417213198E-17,-1.,2.60927675461843E-32));
#24178=DIRECTION('ref_axis',(1.,6.02124417213198E-17,1.51939392966847E-15));
#24179=DIRECTION('',(1.,6.02124417213198E-17,1.51939392966847E-15));
#24180=DIRECTION('',(1.00179694968482E-12,6.02945476819473E-29,-1.));
#24181=DIRECTION('',(1.,6.02124417213198E-17,1.51939392966847E-15));
#24182=DIRECTION('',(1.51939392966847E-15,6.53936508957056E-32,-1.));
#24183=DIRECTION('center_axis',(6.02124417213198E-17,-1.,2.60927675461843E-32));
#24184=DIRECTION('ref_axis',(-1.,-6.02124417213198E-17,-1.51939392966847E-15));
#24185=DIRECTION('center_axis',(6.02124417213198E-17,-1.,2.60927675461843E-32));
#24186=DIRECTION('ref_axis',(-1.,-6.02124417213198E-17,-1.51939392966847E-15));
#24187=DIRECTION('center_axis',(-6.02124417213198E-17,1.,-2.60927675461843E-32));
#24188=DIRECTION('ref_axis',(1.,6.02124417213198E-17,1.51939392966847E-15));
#24189=DIRECTION('center_axis',(6.02124417213198E-17,-1.,2.60927675461843E-32));
#24190=DIRECTION('ref_axis',(1.,6.02124417213198E-17,1.51939392966847E-15));
#24191=DIRECTION('center_axis',(6.02124417213198E-17,-1.,2.60927675461843E-32));
#24192=DIRECTION('ref_axis',(1.,6.02124417213198E-17,1.51939392966847E-15));
#24193=DIRECTION('',(6.02124417213198E-17,-1.,2.60927675461843E-32));
#24194=DIRECTION('center_axis',(6.02124417213198E-17,-1.,2.60927675461843E-32));
#24195=DIRECTION('ref_axis',(1.,6.02124417213198E-17,1.51939392966847E-15));
#24196=DIRECTION('center_axis',(6.02124417213198E-17,-1.,2.60927675461843E-32));
#24197=DIRECTION('ref_axis',(1.,6.02124417213198E-17,1.51939392966847E-15));
#24198=DIRECTION('',(6.02124417213198E-17,-1.,2.60927675461843E-32));
#24199=DIRECTION('center_axis',(6.02124417213198E-17,-1.,2.60927675461843E-32));
#24200=DIRECTION('ref_axis',(-1.,-6.02124417213198E-17,-1.51939392966847E-15));
#24201=DIRECTION('center_axis',(-6.02124417213198E-17,1.,-2.60927675461843E-32));
#24202=DIRECTION('ref_axis',(-1.,-6.02124417213198E-17,-1.51939392966847E-15));
#24203=DIRECTION('',(0.707106781186546,-0.707106781186548,1.1609693565858E-15));
#24204=DIRECTION('center_axis',(-6.02124417213198E-17,1.,-2.60927675461843E-32));
#24205=DIRECTION('ref_axis',(-1.,-6.02124417213198E-17,-1.51939392966847E-15));
#24206=DIRECTION('center_axis',(6.02124417213198E-17,-1.,2.60927675461843E-32));
#24207=DIRECTION('ref_axis',(1.,6.02124417213198E-17,1.51939392966847E-15));
#24208=DIRECTION('center_axis',(6.02124417213198E-17,-1.,2.60927675461843E-32));
#24209=DIRECTION('ref_axis',(1.,6.02124417213198E-17,1.51939392966847E-15));
#24210=DIRECTION('',(6.02124417213198E-17,-1.,2.60927675461843E-32));
#24211=DIRECTION('center_axis',(6.02124417213198E-17,-1.,2.60927675461843E-32));
#24212=DIRECTION('ref_axis',(1.,6.02124417213198E-17,1.51939392966847E-15));
#24213=DIRECTION('center_axis',(6.02124417213198E-17,-1.,2.60927675461843E-32));
#24214=DIRECTION('ref_axis',(1.,6.02124417213198E-17,1.51939392966847E-15));
#24215=DIRECTION('',(6.02124417213198E-17,-1.,2.60927675461843E-32));
#24216=DIRECTION('center_axis',(6.02124417213198E-17,-1.,2.60927675461843E-32));
#24217=DIRECTION('ref_axis',(-0.707106781186546,-4.2576625852945E-17,-0.707106781186549));
#24218=DIRECTION('center_axis',(6.02124417213198E-17,-1.,2.60927675461843E-32));
#24219=DIRECTION('ref_axis',(-0.707106781186546,-4.2576625852945E-17,-0.707106781186549));
#24220=DIRECTION('',(6.02124417213198E-17,-1.,2.60927675461843E-32));
#24221=DIRECTION('center_axis',(-6.02124417213198E-17,1.,-2.60927675461843E-32));
#24222=DIRECTION('ref_axis',(-0.707106781186546,-4.2576625852945E-17,-0.707106781186549));
#24223=DIRECTION('',(-6.02124417213198E-17,1.,-2.60927675461843E-32));
#24224=DIRECTION('center_axis',(-1.31753519791844E-15,-5.32392437742675E-32,
1.));
#24225=DIRECTION('ref_axis',(-6.02124417213198E-17,1.,-2.60927675461841E-32));
#24226=DIRECTION('',(0.0174524064382658,0.999847695156374,2.6517080400408E-17));
#24227=DIRECTION('',(-1.,-6.02124417213198E-17,9.98682464801081E-13));
#24228=DIRECTION('',(-1.,-6.02124417213198E-17,9.98682464801081E-13));
#24229=DIRECTION('center_axis',(6.02124417213198E-17,-1.,2.60927675461843E-32));
#24230=DIRECTION('ref_axis',(1.,6.02124417213198E-17,1.51939392966847E-15));
#24231=DIRECTION('',(-0.707106781186549,-4.25766258529451E-17,0.707106781186546));
#24232=DIRECTION('',(-1.,-6.02124417213198E-17,-1.00165684600473E-12));
#24233=DIRECTION('',(-0.707106781186546,-4.25766258529449E-17,-0.707106781186549));
#24234=DIRECTION('',(1.00165684600473E-12,6.02861116972749E-29,-1.));
#24235=DIRECTION('',(0.707106781186548,4.25766258529451E-17,-0.707106781186547));
#24236=DIRECTION('',(1.,6.02124417213198E-17,1.51939392966847E-15));
#24237=DIRECTION('',(0.707106781186547,4.2576625852945E-17,0.707106781186548));
#24238=DIRECTION('center_axis',(6.02124417213198E-17,-1.,2.60927675461843E-32));
#24239=DIRECTION('ref_axis',(-1.51939392966847E-15,-6.53936508957055E-32,
1.));
#24240=DIRECTION('',(1.,6.02124417213198E-17,-9.98682464801081E-13));
#24241=DIRECTION('center_axis',(6.02124417213198E-17,-1.,2.60927675461843E-32));
#24242=DIRECTION('ref_axis',(1.,6.02124417213198E-17,1.51939392966847E-15));
#24243=DIRECTION('center_axis',(6.02124417213198E-17,-1.,2.60927675461843E-32));
#24244=DIRECTION('ref_axis',(1.,6.02124417213198E-17,1.51939392966847E-15));
#24245=DIRECTION('center_axis',(6.02124417213198E-17,-1.,2.60927675461843E-32));
#24246=DIRECTION('ref_axis',(1.,6.02124417213198E-17,1.51939392966847E-15));
#24247=DIRECTION('center_axis',(6.02124417213198E-17,-1.,2.60927675461843E-32));
#24248=DIRECTION('ref_axis',(1.,6.02124417213198E-17,1.51939392966847E-15));
#24249=DIRECTION('center_axis',(6.02124417213198E-17,-1.,2.60927675461843E-32));
#24250=DIRECTION('ref_axis',(-1.51939392966847E-15,-6.53936508957055E-32,
1.));
#24251=DIRECTION('',(6.02124417213198E-17,-1.,2.60927675461843E-32));
#24252=DIRECTION('center_axis',(-6.02124417213198E-17,1.,-2.60927675461843E-32));
#24253=DIRECTION('ref_axis',(-1.51939392966847E-15,-6.53936508957055E-32,
1.));
#24254=DIRECTION('',(-6.02124417213198E-17,1.,-2.60927675461843E-32));
#24255=DIRECTION('center_axis',(0.707106781186549,4.25766258529451E-17,
-0.707106781186547));
#24256=DIRECTION('ref_axis',(-6.02124417213198E-17,1.,-2.60096122749369E-32));
#24257=DIRECTION('',(6.02124417213198E-17,-1.,2.60927675461843E-32));
#24258=DIRECTION('',(0.707106781186547,4.2576625852945E-17,0.707106781186548));
#24259=DIRECTION('',(-6.02124417213198E-17,1.,-2.60927675461843E-32));
#24260=DIRECTION('',(0.707106781186547,4.2576625852945E-17,0.707106781186548));
#24261=DIRECTION('',(6.02124417213198E-17,-1.,2.60927675461843E-32));
#24262=DIRECTION('',(0.707106781186547,4.2576625852945E-17,0.707106781186548));
#24263=DIRECTION('center_axis',(1.51939392966847E-15,2.46467033119755E-32,
-1.));
#24264=DIRECTION('ref_axis',(1.,-1.41646290028709E-16,1.51939392966847E-15));
#24265=DIRECTION('',(1.,6.02124417213198E-17,-9.98682464801081E-13));
#24266=DIRECTION('',(-0.0174524064382658,-0.999847695156374,-2.6517080400408E-17));
#24267=DIRECTION('center_axis',(0.577350269189625,-0.577350269189626,0.577350269189627));
#24268=DIRECTION('ref_axis',(-1.15783932620466E-15,0.707106781186548,0.707106781186548));
#24269=DIRECTION('',(-1.1169503768152E-15,0.707106781186547,0.707106781186548));
#24270=DIRECTION('',(-0.707106781186546,-0.707106781186549,-1.00421455866691E-12));
#24271=DIRECTION('center_axis',(0.577350269189625,-0.577350269189622,-0.577350269189631));
#24272=DIRECTION('ref_axis',(0.707106781186546,0.707106781186549,9.40034155039792E-16));
#24273=DIRECTION('',(-0.707106781186551,-4.25766258529452E-17,-0.707106781186544));
#24274=DIRECTION('',(0.707106781186546,0.707106781186549,1.07437375096225E-15));
#24275=DIRECTION('center_axis',(0.707106781186544,4.25766258529448E-17,
-0.707106781186551));
#24276=DIRECTION('ref_axis',(-6.02124417213198E-17,1.,-2.25152429480529E-32));
#24277=DIRECTION('',(0.707106781186551,4.25766258529452E-17,0.707106781186544));
#24278=DIRECTION('',(6.02124417213198E-17,-1.,2.60927675461843E-32));
#24279=DIRECTION('center_axis',(0.707106781186549,-0.707106781186546,1.27063530829773E-15));
#24280=DIRECTION('ref_axis',(-1.51939392966847E-15,2.77555756156293E-16,
1.));
#24281=DIRECTION('',(-1.00179694968482E-12,-6.02945476819473E-29,1.));
#24282=DIRECTION('center_axis',(-1.03179712510931E-15,-0.707106781186548,
0.707106781186547));
#24283=DIRECTION('ref_axis',(-1.,-6.02124417213168E-17,-1.51939392966847E-15));
#24284=DIRECTION('',(-1.,-6.02124417213198E-17,-1.51939392966847E-15));
#24285=DIRECTION('',(0.0123416547519181,0.707052927141238,0.707052927141238));
#24286=DIRECTION('',(0.584067929597371,0.573961955888994,0.573961955888995));
#24287=DIRECTION('center_axis',(6.02124417213198E-17,-1.,2.60927675461843E-32));
#24288=DIRECTION('ref_axis',(-0.707106781186548,-4.25766258529451E-17,-0.707106781186547));
#24289=DIRECTION('center_axis',(-6.02124417213198E-17,1.,-2.60927675461843E-32));
#24290=DIRECTION('ref_axis',(-0.707106781186548,-4.25766258529451E-17,-0.707106781186547));
#24291=DIRECTION('',(-6.02124417213198E-17,1.,-2.60927675461843E-32));
#24292=DIRECTION('center_axis',(-6.02124417213198E-17,1.,-2.60927675461843E-32));
#24293=DIRECTION('ref_axis',(-0.707106781186548,-4.25766258529451E-17,-0.707106781186547));
#24294=DIRECTION('',(6.02124417213198E-17,-1.,2.60927675461843E-32));
#24295=DIRECTION('center_axis',(1.51939392966847E-15,6.53936508957056E-32,
-1.));
#24296=DIRECTION('ref_axis',(1.,6.02124417213198E-17,1.51939392966847E-15));
#24297=DIRECTION('',(1.,6.02124417213198E-17,1.51939392966847E-15));
#24298=DIRECTION('',(6.02124417213198E-17,-1.,2.60927675461843E-32));
#24299=DIRECTION('',(1.,6.02124417213198E-17,1.51939392966847E-15));
#24300=DIRECTION('center_axis',(6.02124417213198E-17,-1.,2.60927675461843E-32));
#24301=DIRECTION('ref_axis',(0.707106781186547,4.2576625852945E-17,-0.707106781186548));
#24302=DIRECTION('center_axis',(-6.02124417213198E-17,1.,-2.60927675461843E-32));
#24303=DIRECTION('ref_axis',(0.707106781186547,4.2576625852945E-17,-0.707106781186548));
#24304=DIRECTION('',(-6.02124417213198E-17,1.,-2.60927675461843E-32));
#24305=DIRECTION('center_axis',(-6.02124417213198E-17,1.,-2.60927675461843E-32));
#24306=DIRECTION('ref_axis',(0.707106781186547,4.2576625852945E-17,-0.707106781186548));
#24307=DIRECTION('center_axis',(1.,6.02124417213198E-17,1.51939392966847E-15));
#24308=DIRECTION('ref_axis',(6.02124417213198E-17,-1.,2.60927675461843E-32));
#24309=DIRECTION('',(-1.51939392966847E-15,-6.53936508957056E-32,1.));
#24310=DIRECTION('',(6.02124417213198E-17,-1.,2.60927675461843E-32));
#24311=DIRECTION('',(-1.51939392966847E-15,-6.53936508957056E-32,1.));
#24312=DIRECTION('center_axis',(6.02124417213198E-17,-1.,2.60927675461843E-32));
#24313=DIRECTION('ref_axis',(0.707106781186545,4.25766258529449E-17,0.70710678118655));
#24314=DIRECTION('center_axis',(-6.02124417213198E-17,1.,-2.60927675461843E-32));
#24315=DIRECTION('ref_axis',(0.707106781186545,4.25766258529449E-17,0.70710678118655));
#24316=DIRECTION('',(-6.02124417213198E-17,1.,-2.60927675461843E-32));
#24317=DIRECTION('center_axis',(-6.02124417213198E-17,1.,-2.60927675461843E-32));
#24318=DIRECTION('ref_axis',(0.707106781186545,4.25766258529449E-17,0.70710678118655));
#24319=DIRECTION('center_axis',(-1.51939392966847E-15,-6.53936508957056E-32,
1.));
#24320=DIRECTION('ref_axis',(-6.02124417213198E-17,1.,-2.60927675461842E-32));
#24321=DIRECTION('',(-1.,-6.02124417213198E-17,-1.51939392966847E-15));
#24322=DIRECTION('',(6.02124417213198E-17,-1.,2.60927675461843E-32));
#24323=DIRECTION('',(-1.,-6.02124417213198E-17,-1.51939392966847E-15));
#24324=DIRECTION('center_axis',(6.02124417213198E-17,-1.,2.60927675461843E-32));
#24325=DIRECTION('ref_axis',(-0.707106781186547,-4.2576625852945E-17,0.707106781186548));
#24326=DIRECTION('center_axis',(-6.02124417213198E-17,1.,-2.60927675461843E-32));
#24327=DIRECTION('ref_axis',(-0.707106781186547,-4.2576625852945E-17,0.707106781186548));
#24328=DIRECTION('',(-6.02124417213198E-17,1.,-2.60927675461843E-32));
#24329=DIRECTION('center_axis',(-6.02124417213198E-17,1.,-2.60927675461843E-32));
#24330=DIRECTION('ref_axis',(-0.707106781186547,-4.2576625852945E-17,0.707106781186548));
#24331=DIRECTION('center_axis',(6.02124417213198E-17,-1.,2.60927675461843E-32));
#24332=DIRECTION('ref_axis',(1.,6.02124417213198E-17,1.51939392966847E-15));
#24333=DIRECTION('',(1.51939392966847E-15,6.53936508957056E-32,-1.));
#24334=DIRECTION('center_axis',(-1.,-6.02124417213198E-17,-1.51939392966847E-15));
#24335=DIRECTION('ref_axis',(1.51939392966847E-15,6.53936508957056E-32,
-1.));
#24336=DIRECTION('',(1.51939392966847E-15,6.53936508957056E-32,-1.));
#24337=DIRECTION('center_axis',(0.999847695156391,-0.0174524064372835,1.51916251861363E-15));
#24338=DIRECTION('ref_axis',(-1.51939392966847E-15,-9.04549301518072E-32,
1.));
#24339=DIRECTION('center_axis',(0.700909264299845,-0.713250449154187,1.06495728142558E-15));
#24340=DIRECTION('ref_axis',(-1.51939392966847E-15,1.65690546530681E-30,
1.));
#24341=DIRECTION('',(-1.51939392966847E-15,-6.53936508957056E-32,1.));
#24342=DIRECTION('center_axis',(6.02124417213198E-17,-1.,2.60927675461843E-32));
#24343=DIRECTION('ref_axis',(1.,6.02124417213198E-17,1.51939392966847E-15));
#24344=DIRECTION('center_axis',(6.02124417213198E-17,-1.,2.60927675461843E-32));
#24345=DIRECTION('ref_axis',(1.,6.02124417213198E-17,1.51939392966847E-15));
#24346=DIRECTION('',(6.02124417213198E-17,-1.,2.60927675461843E-32));
#24347=DIRECTION('center_axis',(-1.51939392966847E-15,-6.53936508957056E-32,
1.));
#24348=DIRECTION('ref_axis',(-6.02124417213198E-17,1.,-2.60927675461842E-32));
#24349=DIRECTION('',(-1.,-6.02124417213198E-17,-1.51939392966847E-15));
#24350=DIRECTION('',(0.0174524064382658,0.999847695156374,2.6517080400408E-17));
#24351=DIRECTION('center_axis',(1.,6.02124417213198E-17,1.79694968582476E-15));
#24352=DIRECTION('ref_axis',(6.02124417213198E-17,-1.,2.60927675461843E-32));
#24353=DIRECTION('',(-1.00179694968482E-12,-6.02945476819473E-29,1.));
#24354=DIRECTION('center_axis',(-6.02124417213198E-17,1.,-2.60927675461843E-32));
#24355=DIRECTION('ref_axis',(0.0161939654040152,9.75078198126308E-19,-0.999868869144596));
#24356=DIRECTION('center_axis',(6.02124417213198E-17,-1.,2.60927675461843E-32));
#24357=DIRECTION('ref_axis',(0.0161939654068418,9.75078198296505E-19,-0.99986886914455));
#24358=DIRECTION('',(6.02124417213198E-17,-1.,2.60927675461843E-32));
#24359=DIRECTION('center_axis',(-6.02124417213198E-17,1.,-2.60927675461843E-32));
#24360=DIRECTION('ref_axis',(0.0161939654068418,9.75078198296505E-19,-0.99986886914455));
#24361=DIRECTION('',(-6.02124417213198E-17,1.,-2.60927675461843E-32));
#24362=DIRECTION('center_axis',(-6.02124417213198E-17,1.,-2.60927675461843E-32));
#24363=DIRECTION('ref_axis',(-1.51939392966847E-15,-6.53936508957055E-32,
1.));
#24364=DIRECTION('',(-0.707106781186549,-4.25766258529451E-17,0.707106781186546));
#24365=DIRECTION('center_axis',(-6.02124417213198E-17,1.,-2.60927675461843E-32));
#24366=DIRECTION('ref_axis',(-0.999868869144596,-6.02045460123309E-17,-0.0161939654040152));
#24367=DIRECTION('center_axis',(6.02124417213198E-17,-1.,2.60927675461843E-32));
#24368=DIRECTION('ref_axis',(-0.99986886914455,-6.02045460123282E-17,-0.0161939654068418));
#24369=DIRECTION('center_axis',(-6.02124417213198E-17,1.,-2.60927675461843E-32));
#24370=DIRECTION('ref_axis',(-0.99986886914455,-6.02045460123282E-17,-0.0161939654068418));
#24371=DIRECTION('center_axis',(-6.02124417213198E-17,1.,-2.60927675461843E-32));
#24372=DIRECTION('ref_axis',(-1.51939392966847E-15,-6.53936508957055E-32,
1.));
#24373=DIRECTION('center_axis',(-6.02124417213198E-17,1.,-2.60927675461843E-32));
#24374=DIRECTION('ref_axis',(-0.0161939654040153,-9.75078198126314E-19,
0.999868869144596));
#24375=DIRECTION('center_axis',(6.02124417213198E-17,-1.,2.60927675461843E-32));
#24376=DIRECTION('ref_axis',(-0.0161939654068419,-9.75078198296511E-19,
0.99986886914455));
#24377=DIRECTION('',(6.02124417213198E-17,-1.,2.60927675461843E-32));
#24378=DIRECTION('center_axis',(-6.02124417213198E-17,1.,-2.60927675461843E-32));
#24379=DIRECTION('ref_axis',(-0.0161939654068419,-9.75078198296511E-19,
0.99986886914455));
#24380=DIRECTION('',(-6.02124417213198E-17,1.,-2.60927675461843E-32));
#24381=DIRECTION('center_axis',(-6.02124417213198E-17,1.,-2.60927675461843E-32));
#24382=DIRECTION('ref_axis',(-1.51939392966847E-15,-6.53936508957055E-32,
1.));
#24383=DIRECTION('',(0.707106781186548,4.25766258529451E-17,-0.707106781186547));
#24384=DIRECTION('center_axis',(0.707106781186546,4.25766258529449E-17,
0.707106781186549));
#24385=DIRECTION('ref_axis',(-6.02124417213198E-17,1.,1.32224183220761E-32));
#24386=DIRECTION('',(-0.707106781186549,-4.25766258529451E-17,0.707106781186546));
#24387=DIRECTION('',(-0.707106781186549,-4.25766258529451E-17,0.707106781186546));
#24388=DIRECTION('',(6.02124417213198E-17,-1.,2.60927675461843E-32));
#24389=DIRECTION('center_axis',(-0.707106781186547,-4.2576625852945E-17,
-0.707106781186549));
#24390=DIRECTION('ref_axis',(6.02124417213198E-17,-1.,9.64348767934759E-33));
#24391=DIRECTION('',(0.707106781186548,4.25766258529451E-17,-0.707106781186547));
#24392=DIRECTION('',(6.02124417213198E-17,-1.,2.60927675461843E-32));
#24393=DIRECTION('',(6.02124417213198E-17,-1.,2.60927675461843E-32));
#24394=DIRECTION('',(0.707106781186548,4.25766258529451E-17,-0.707106781186547));
#24395=DIRECTION('center_axis',(-6.02124417213198E-17,1.,-2.60927675461843E-32));
#24396=DIRECTION('ref_axis',(0.999868869144596,6.02045460123309E-17,0.0161939654040153));
#24397=DIRECTION('center_axis',(6.02124417213198E-17,-1.,2.60927675461843E-32));
#24398=DIRECTION('ref_axis',(0.99986886914455,6.02045460123282E-17,0.0161939654068419));
#24399=DIRECTION('',(6.02124417213198E-17,-1.,2.60927675461843E-32));
#24400=DIRECTION('center_axis',(-6.02124417213198E-17,1.,-2.60927675461843E-32));
#24401=DIRECTION('ref_axis',(0.99986886914455,6.02045460123282E-17,0.0161939654068419));
#24402=DIRECTION('',(-6.02124417213198E-17,1.,-2.60927675461843E-32));
#24403=DIRECTION('center_axis',(-6.02124417213198E-17,1.,-2.60927675461843E-32));
#24404=DIRECTION('ref_axis',(-1.51939392966847E-15,-6.53936508957055E-32,
1.));
#24405=DIRECTION('',(-0.707106781186546,-4.25766258529449E-17,-0.707106781186549));
#24406=DIRECTION('center_axis',(-0.707106781186549,-4.25766258529451E-17,
0.707106781186546));
#24407=DIRECTION('ref_axis',(-0.707106781186546,-4.25766258529449E-17,-0.707106781186549));
#24408=DIRECTION('',(-0.707106781186546,-4.25766258529449E-17,-0.707106781186549));
#24409=DIRECTION('',(6.02124417213198E-17,-1.,2.60927675461843E-32));
#24410=DIRECTION('',(6.02124417213198E-17,-1.,2.60927675461843E-32));
#24411=DIRECTION('',(-0.707106781186546,-4.25766258529449E-17,-0.707106781186549));
#24412=DIRECTION('center_axis',(-1.02201073032319E-15,-0.713250449154181,
0.700909264299851));
#24413=DIRECTION('ref_axis',(-1.,-6.02124417213166E-17,-1.51939392966847E-15));
#24414=DIRECTION('center_axis',(6.02124417213198E-17,-1.,2.60927675461843E-32));
#24415=DIRECTION('ref_axis',(-1.,-6.02124417213198E-17,-1.51939392966847E-15));
#24416=DIRECTION('center_axis',(-6.02124417213198E-17,1.,-2.60927675461843E-32));
#24417=DIRECTION('ref_axis',(-1.,-6.02124417213198E-17,-1.51939392966847E-15));
#24418=DIRECTION('',(-0.707106781186546,0.707106781186549,-1.1609693565858E-15));
#24419=DIRECTION('center_axis',(6.02124417213198E-17,-1.,2.60927675461843E-32));
#24420=DIRECTION('ref_axis',(-1.,-6.02124417213198E-17,-1.51939392966847E-15));
#24421=DIRECTION('center_axis',(-6.02124417213198E-17,1.,-2.60927675461843E-32));
#24422=DIRECTION('ref_axis',(-1.51939392966847E-15,-6.53936508957055E-32,
1.));
#24423=DIRECTION('center_axis',(-6.02124417213198E-17,1.,-2.60927675461843E-32));
#24424=DIRECTION('ref_axis',(-1.,-6.02124417213198E-17,-1.51939392966847E-15));
#24425=DIRECTION('center_axis',(6.02124417213198E-17,-1.,2.60927675461843E-32));
#24426=DIRECTION('ref_axis',(-1.,-6.02124417213198E-17,-1.51939392966847E-15));
#24427=DIRECTION('center_axis',(-6.02124417213198E-17,1.,-2.60927675461843E-32));
#24428=DIRECTION('ref_axis',(-1.,-6.02124417213198E-17,-1.51939392966847E-15));
#24429=DIRECTION('',(-6.02124417213198E-17,1.,-2.60927675461843E-32));
#24430=DIRECTION('center_axis',(-6.02124417213198E-17,1.,-2.60927675461843E-32));
#24431=DIRECTION('ref_axis',(-1.,-6.02124417213198E-17,-1.51939392966847E-15));
#24432=DIRECTION('center_axis',(6.02124417213198E-17,-1.,2.60927675461843E-32));
#24433=DIRECTION('ref_axis',(-1.,-6.02124417213198E-17,-1.51939392966847E-15));
#24434=DIRECTION('',(0.242535625036333,0.970142500145332,3.38805108720557E-16));
#24435=DIRECTION('center_axis',(6.02124417213198E-17,-1.,2.60927675461843E-32));
#24436=DIRECTION('ref_axis',(-1.,-6.02124417213198E-17,-1.51939392966847E-15));
#24437=DIRECTION('center_axis',(6.02124417213198E-17,-1.,2.60927675461843E-32));
#24438=DIRECTION('ref_axis',(1.,6.02124417213198E-17,1.51939392966847E-15));
#24439=DIRECTION('',(6.02124417213198E-17,-1.,2.60927675461843E-32));
#24440=DIRECTION('center_axis',(6.02124417213198E-17,-1.,2.60927675461843E-32));
#24441=DIRECTION('ref_axis',(1.,6.02124417213198E-17,1.51939392966847E-15));
#24442=DIRECTION('center_axis',(6.02124417213198E-17,-1.,2.60927675461843E-32));
#24443=DIRECTION('ref_axis',(1.,6.02124417213198E-17,1.51939392966847E-15));
#24444=DIRECTION('center_axis',(6.02124417213198E-17,-1.,2.60927675461843E-32));
#24445=DIRECTION('ref_axis',(1.,6.02124417213198E-17,1.51939392966847E-15));
#24446=DIRECTION('center_axis',(6.02124417213198E-17,-1.,2.60927675461843E-32));
#24447=DIRECTION('ref_axis',(1.,6.02124417213198E-17,1.51939392966847E-15));
#24448=DIRECTION('',(6.02124417213198E-17,-1.,2.60927675461843E-32));
#24449=DIRECTION('center_axis',(6.02124417213198E-17,-1.,2.60927675461843E-32));
#24450=DIRECTION('ref_axis',(1.,6.02124417213198E-17,1.51939392966847E-15));
#24451=DIRECTION('center_axis',(6.02124417213198E-17,-1.,2.60927675461843E-32));
#24452=DIRECTION('ref_axis',(1.,6.02124417213198E-17,1.51939392966847E-15));
#24453=DIRECTION('center_axis',(6.02124417213198E-17,-1.,2.60927675461843E-32));
#24454=DIRECTION('ref_axis',(1.,6.02124417213198E-17,1.51939392966847E-15));
#24455=DIRECTION('',(6.02124417213198E-17,-1.,2.60927675461843E-32));
#24456=DIRECTION('center_axis',(6.02124417213198E-17,-1.,2.60927675461843E-32));
#24457=DIRECTION('ref_axis',(1.,6.02124417213198E-17,1.51939392966847E-15));
#24458=DIRECTION('center_axis',(6.02124417213198E-17,-1.,2.60927675461843E-32));
#24459=DIRECTION('ref_axis',(1.,6.02124417213198E-17,1.51939392966847E-15));
#24460=DIRECTION('center_axis',(6.02124417213198E-17,-1.,2.60927675461843E-32));
#24461=DIRECTION('ref_axis',(1.,6.02124417213198E-17,1.51939392966847E-15));
#24462=DIRECTION('',(6.02124417213198E-17,-1.,2.60927675461843E-32));
#24463=DIRECTION('center_axis',(6.02124417213198E-17,-1.,2.60927675461843E-32));
#24464=DIRECTION('ref_axis',(1.,6.02124417213198E-17,1.51939392966847E-15));
#24465=DIRECTION('center_axis',(6.02124417213198E-17,-1.,2.60927675461843E-32));
#24466=DIRECTION('ref_axis',(1.,6.02124417213198E-17,1.51939392966847E-15));
#24467=DIRECTION('center_axis',(6.02124417213198E-17,-1.,2.60927675461843E-32));
#24468=DIRECTION('ref_axis',(1.,6.02124417213198E-17,1.51939392966847E-15));
#24469=DIRECTION('',(6.02124417213198E-17,-1.,2.60927675461843E-32));
#24470=DIRECTION('center_axis',(-6.02124417213198E-17,1.,-2.60927675461843E-32));
#24471=DIRECTION('ref_axis',(-1.51939392966847E-15,-6.53936508957055E-32,
1.));
#24472=DIRECTION('',(1.,6.02124417213198E-17,1.51939392966847E-15));
#24473=DIRECTION('',(1.00165684600473E-12,6.02861116972749E-29,-1.));
#24474=DIRECTION('',(-1.,-6.02124417213198E-17,-1.00165684600473E-12));
#24475=DIRECTION('center_axis',(6.02124417213198E-17,-1.,2.60927675461843E-32));
#24476=DIRECTION('ref_axis',(1.,6.02124417213198E-17,1.51939392966847E-15));
#24477=DIRECTION('center_axis',(6.02124417213198E-17,-1.,2.60927675461843E-32));
#24478=DIRECTION('ref_axis',(1.,6.02124417213198E-17,1.51939392966847E-15));
#24479=DIRECTION('',(6.02124417213198E-17,-1.,2.60927675461843E-32));
#24480=DIRECTION('center_axis',(6.02124417213198E-17,-1.,2.60927675461843E-32));
#24481=DIRECTION('ref_axis',(1.,6.02124417213198E-17,1.51939392966847E-15));
#24482=DIRECTION('center_axis',(-6.02124417213198E-17,1.,-2.60927675461843E-32));
#24483=DIRECTION('ref_axis',(-1.51939392966847E-15,-6.53936508957055E-32,
1.));
#24484=DIRECTION('center_axis',(-6.02124417213198E-17,1.,-2.60927675461843E-32));
#24485=DIRECTION('ref_axis',(-1.51939392966847E-15,-6.53936508957055E-32,
1.));
#24486=DIRECTION('center_axis',(1.51939392966847E-15,6.53936508957056E-32,
-1.));
#24487=DIRECTION('ref_axis',(1.,6.02124417213198E-17,1.51939392966847E-15));
#24488=DIRECTION('center_axis',(-1.,-6.02124417213198E-17,-1.6568460057356E-15));
#24489=DIRECTION('ref_axis',(6.02124417213198E-17,-1.,2.60927675461843E-32));
#24490=DIRECTION('center_axis',(-1.6568460057356E-15,-7.36699760153718E-32,
1.));
#24491=DIRECTION('ref_axis',(-1.,-6.02124417213198E-17,-1.6568460057356E-15));
#24492=DIRECTION('center_axis',(0.999847695156391,-0.0174524064372835,1.51916251861363E-15));
#24493=DIRECTION('ref_axis',(-1.51939392966847E-15,-9.04549301518072E-32,
1.));
#24494=DIRECTION('axis',(0.,0.,1.));
#24495=DIRECTION('refdir',(1.,0.,0.));
#24496=DIRECTION('center_axis',(6.12323404134149E-17,-1.,3.14444500472474E-32));
#24497=DIRECTION('ref_axis',(1.55749764652046E-5,0.,-0.99999999987871));
#24498=DIRECTION('center_axis',(-6.12323404134149E-17,1.,-3.14444500472474E-32));
#24499=DIRECTION('ref_axis',(-0.99999999987871,-6.1232340405988E-17,-1.55749751705838E-5));
#24500=DIRECTION('center_axis',(-0.99999999987871,-6.12323404059881E-17,
-1.55749764653271E-5));
#24501=DIRECTION('ref_axis',(-1.55749764653271E-5,0.,0.99999999987871));
#24502=DIRECTION('center_axis',(6.12323404134149E-17,-1.,3.14444500472474E-32));
#24503=DIRECTION('ref_axis',(-0.99999999987871,-6.12323404059881E-17,-1.55749752150822E-5));
#24504=DIRECTION('center_axis',(6.12323404134149E-17,-1.,3.14444500472474E-32));
#24505=DIRECTION('ref_axis',(-0.99999999987871,-6.12323404059881E-17,-1.55749752150822E-5));
#24506=DIRECTION('center_axis',(6.12323404134149E-17,-1.,3.14444500472474E-32));
#24507=DIRECTION('ref_axis',(0.99999999987871,6.12323404059881E-17,1.55749764652046E-5));
#24508=DIRECTION('',(-6.12323404134149E-17,1.,-3.14444500472474E-32));
#24509=DIRECTION('center_axis',(-6.12323404134149E-17,1.,-3.14444500472474E-32));
#24510=DIRECTION('ref_axis',(-0.99999999987871,-6.12323404059881E-17,-1.55749752150822E-5));
#24511=DIRECTION('center_axis',(-6.12323404134149E-17,1.,-3.14444500472474E-32));
#24512=DIRECTION('ref_axis',(-0.99999999987871,-6.12323404059881E-17,-1.55749752150822E-5));
#24513=DIRECTION('center_axis',(6.12323404134149E-17,-1.,3.14444500472474E-32));
#24514=DIRECTION('ref_axis',(0.99999999987871,6.12323404059881E-17,1.55749764652046E-5));
#24515=DIRECTION('center_axis',(6.12323404134149E-17,-1.,3.14444500472474E-32));
#24516=DIRECTION('ref_axis',(0.99999999987871,6.1232340405988E-17,1.55749764652046E-5));
#24517=DIRECTION('center_axis',(6.12323404134149E-17,-1.,3.14444500472474E-32));
#24518=DIRECTION('ref_axis',(1.55749764652046E-5,0.,-0.99999999987871));
#24519=DIRECTION('center_axis',(-0.99999999987871,-6.12323404059881E-17,
-1.55749764653271E-5));
#24520=DIRECTION('ref_axis',(-1.55749764653271E-5,0.,0.99999999987871));
#24521=DIRECTION('center_axis',(6.12323404134149E-17,-1.,3.14444500472474E-32));
#24522=DIRECTION('ref_axis',(-0.99999999987871,-6.1232340405988E-17,-1.55749751705838E-5));
#24523=DIRECTION('center_axis',(-6.12323404134149E-17,1.,-3.14444500472474E-32));
#24524=DIRECTION('ref_axis',(-1.55749764652046E-5,-9.53692260816889E-22,
0.99999999987871));
#24525=DIRECTION('center_axis',(6.12323404134149E-17,-1.,3.14444500472474E-32));
#24526=DIRECTION('ref_axis',(0.99999999987871,6.1232340405988E-17,1.55749764652046E-5));
#24527=DIRECTION('center_axis',(6.12323404134149E-17,-1.,3.14444500472474E-32));
#24528=DIRECTION('ref_axis',(0.99999999987871,6.1232340405988E-17,1.55749764652046E-5));
#24529=DIRECTION('',(6.12323404134149E-17,-1.,3.14444500472474E-32));
#24530=DIRECTION('axis',(0.,0.,1.));
#24531=DIRECTION('refdir',(1.,0.,0.));
#24532=DIRECTION('center_axis',(1.,5.1420277733694E-16,-1.0522467400333E-14));
#24533=DIRECTION('ref_axis',(-1.0522467400333E-14,1.06077175752244E-14,
-1.));
#24534=DIRECTION('',(-1.00001914094642E-12,1.00002200370999E-12,1.));
#24535=DIRECTION('',(9.99479153109778E-13,1.,-9.99999999999011E-13));
#24536=DIRECTION('',(1.00001914094642E-12,-9.99999999998997E-13,-1.));
#24537=DIRECTION('',(-9.47915311079142E-15,-1.,1.E-14));
#24538=DIRECTION('center_axis',(-4.5961454925099E-16,1.,6.61092274672771E-17));
#24539=DIRECTION('ref_axis',(-1.05885766278003E-14,6.61092274672722E-17,
-1.));
#24540=DIRECTION('',(1.,-9.54038545074888E-15,9.9999999999998E-15));
#24541=DIRECTION('',(-9.56631913100564E-15,9.99999999999985E-15,1.));
#24542=DIRECTION('',(-1.,9.54038545074888E-15,-9.9999999999998E-15));
#24543=DIRECTION('center_axis',(0.,-4.29362650667545E-31,1.));
#24544=DIRECTION('ref_axis',(4.28756753891971E-16,-1.,-4.29362650667545E-31));
#24545=DIRECTION('',(-9.99999999999976E-15,-1.04336808689941E-14,1.));
#24546=DIRECTION('center_axis',(-1.99999999991998E-11,2.E-11,1.));
#24547=DIRECTION('ref_axis',(-1.99995712428458E-11,-1.,1.99999999996E-11));
#24548=DIRECTION('',(-9.56631913100564E-15,9.99999999999985E-15,1.));
#24549=DIRECTION('center_axis',(-1.99999999991998E-11,2.E-11,1.));
#24550=DIRECTION('ref_axis',(-1.99995712428458E-11,-1.,1.99999999996E-11));
#24551=DIRECTION('center_axis',(1.,5.2084688920845E-16,-1.0522467400333E-14));
#24552=DIRECTION('ref_axis',(-1.0522467400333E-14,1.01548957588061E-14,
-1.));
#24553=DIRECTION('',(-9.47915311079142E-15,-1.,1.E-14));
#24554=DIRECTION('',(-9.47915311079142E-15,-1.,1.E-14));
#24555=DIRECTION('center_axis',(-1.0522467400333E-14,-2.20037109949262E-17,
-1.));
#24556=DIRECTION('ref_axis',(1.,-6.86759532082262E-15,-1.0522467400333E-14));
#24557=DIRECTION('',(-1.,9.99485333130104E-13,-9.99628143109513E-13));
#24558=DIRECTION('',(9.99479153109778E-13,1.,-1.00002200371E-12));
#24559=DIRECTION('',(1.,-9.99466108488984E-13,1.00024333162532E-12));
#24560=DIRECTION('center_axis',(5.33891510011771E-16,-1.,2.20037109950003E-17));
#24561=DIRECTION('ref_axis',(-1.,-5.33891510011771E-16,1.0522467400333E-14));
#24562=DIRECTION('',(9.99999999998993E-13,-1.00002200370999E-12,-1.));
#24563=DIRECTION('',(1.,-9.99466108488984E-13,1.00024333162532E-12));
#24564=DIRECTION('center_axis',(-2.43331626335201E-16,2.20037109950001E-17,
1.));
#24565=DIRECTION('ref_axis',(1.,3.89820370584558E-15,2.43331626335201E-16));
#24566=DIRECTION('',(-9.99479153109778E-13,-1.,1.00002200371E-12));
#24567=DIRECTION('',(1.,-9.99466108488984E-13,1.00024333162532E-12));
#24568=DIRECTION('center_axis',(-5.3389151001177E-16,1.,6.61092274672778E-17));
#24569=DIRECTION('ref_axis',(-1.06105803387953E-14,6.61092274672721E-17,
-1.));
#24570=DIRECTION('',(-9.99999999998993E-13,1.00002200370999E-12,1.));
#24571=DIRECTION('center_axis',(1.,5.33891510011885E-16,-1.0522467400333E-14));
#24572=DIRECTION('ref_axis',(-1.0522467400333E-14,1.08319082541355E-14,
-1.));
#24573=DIRECTION('axis',(0.,0.,1.));
#24574=DIRECTION('refdir',(1.,0.,0.));
#24575=DIRECTION('center_axis',(1.,5.2084688920845E-16,-1.0522467400333E-14));
#24576=DIRECTION('ref_axis',(-1.0522467400333E-14,1.01548957588061E-14,
-1.));
#24577=DIRECTION('',(-9.56631913100564E-15,9.99999999999985E-15,1.));
#24578=DIRECTION('',(-9.47915311079142E-15,-1.,1.E-14));
#24579=DIRECTION('',(-9.56631913100564E-15,9.99999999999985E-15,1.));
#24580=DIRECTION('',(-9.47915311079142E-15,-1.,1.E-14));
#24581=DIRECTION('center_axis',(0.,3.71824206197546E-31,1.));
#24582=DIRECTION('ref_axis',(1.,3.89820370584558E-15,-1.44944649852236E-45));
#24583=DIRECTION('center_axis',(-1.99999999991998E-11,2.E-11,1.));
#24584=DIRECTION('ref_axis',(-1.99995712428458E-11,-1.,1.99999999996E-11));
#24585=DIRECTION('',(1.,-9.54038545074888E-15,9.9999999999998E-15));
#24586=DIRECTION('',(-9.47915311079142E-15,-1.,1.E-14));
#24587=DIRECTION('',(1.,-9.99466108488984E-13,1.00024333162532E-12));
#24588=DIRECTION('',(-9.99479153109778E-13,-1.,1.0044628958085E-12));
#24589=DIRECTION('',(1.,-9.99466108488984E-13,1.00024333162532E-12));
#24590=DIRECTION('center_axis',(0.,-4.29362650667545E-31,1.));
#24591=DIRECTION('ref_axis',(4.28756753891971E-16,-1.,-4.29362650667545E-31));
#24592=DIRECTION('',(-9.99999999999976E-15,-1.04336808689941E-14,1.));
#24593=DIRECTION('center_axis',(-1.99999999991998E-11,2.E-11,1.));
#24594=DIRECTION('ref_axis',(-1.99995712428458E-11,-1.,1.99999999996E-11));
#24595=DIRECTION('center_axis',(-1.0522467400333E-14,6.93088260946523E-29,
-1.));
#24596=DIRECTION('ref_axis',(1.,-6.62426369448742E-15,-1.0522467400333E-14));
#24597=DIRECTION('',(-9.47915311079142E-15,-1.,1.E-14));
#24598=DIRECTION('',(-1.,9.54038545074888E-15,-9.9999999999998E-15));
#24599=DIRECTION('',(-1.,9.99485333130104E-13,-9.99628143109513E-13));
#24600=DIRECTION('',(9.99479153109778E-13,1.,-1.00002200371E-12));
#24601=DIRECTION('',(1.,-9.99466108488984E-13,1.00024333162532E-12));
#24602=DIRECTION('center_axis',(-4.5961454925099E-16,1.,6.61092274672771E-17));
#24603=DIRECTION('ref_axis',(-1.05885766278003E-14,6.61092274672722E-17,
-1.));
#24604=DIRECTION('',(1.00001914094642E-12,-9.99999999998997E-13,-1.));
#24605=DIRECTION('center_axis',(1.,5.1420277733694E-16,-1.0522467400333E-14));
#24606=DIRECTION('ref_axis',(-1.0522467400333E-14,1.06077175752244E-14,
-1.));
#24607=DIRECTION('',(-1.00001914094642E-12,1.00002200370999E-12,1.));
#24608=DIRECTION('center_axis',(5.33891510011771E-16,-1.,2.20037109950003E-17));
#24609=DIRECTION('ref_axis',(-1.,-5.33891510011771E-16,1.0522467400333E-14));
#24610=DIRECTION('',(9.99999999998993E-13,-1.00002200370999E-12,-1.));
#24611=DIRECTION('center_axis',(-5.3389151001177E-16,1.,6.61092274672778E-17));
#24612=DIRECTION('ref_axis',(-1.06105803387953E-14,6.61092274672721E-17,
-1.));
#24613=DIRECTION('',(-9.99999999998993E-13,1.00002200370999E-12,1.));
#24614=DIRECTION('center_axis',(1.,5.33891510011885E-16,-1.0522467400333E-14));
#24615=DIRECTION('ref_axis',(-1.0522467400333E-14,1.08319082541355E-14,
-1.));
#24616=DIRECTION('axis',(0.,0.,1.));
#24617=DIRECTION('refdir',(1.,0.,0.));
#24618=DIRECTION('center_axis',(2.07638679158937E-16,-1.,1.20948400507518E-31));
#24619=DIRECTION('ref_axis',(0.00551570721125935,1.14527415997344E-18,0.999984788371283));
#24620=DIRECTION('center_axis',(-2.07638679158937E-16,1.,-1.20948400507518E-31));
#24621=DIRECTION('ref_axis',(0.792981602406797,1.64653652521085E-16,-0.609245581226774));
#24622=DIRECTION('',(2.07638679158937E-16,-1.,1.20948400507518E-31));
#24623=DIRECTION('center_axis',(2.07638679158937E-16,-1.,1.20948400507518E-31));
#24624=DIRECTION('ref_axis',(0.792981602406797,1.64653652521085E-16,-0.609245581226774));
#24625=DIRECTION('',(2.07638679158937E-16,-1.,1.20948400507518E-31));
#24626=DIRECTION('center_axis',(2.07638679158937E-16,-1.,1.20948400507518E-31));
#24627=DIRECTION('ref_axis',(-0.944120330982807,-1.96035898492368E-16,-0.329600971820345));
#24628=DIRECTION('center_axis',(-2.07638679158937E-16,1.,-1.20948400507518E-31));
#24629=DIRECTION('ref_axis',(-0.944120330979384,-1.96035898491658E-16,-0.329600971830149));
#24630=DIRECTION('',(2.07638679158937E-16,-1.,1.20948400507518E-31));
#24631=DIRECTION('center_axis',(2.07638679158937E-16,-1.,1.20948400507518E-31));
#24632=DIRECTION('ref_axis',(-0.944120330979384,-1.96035898491658E-16,-0.329600971830149));
#24633=DIRECTION('center_axis',(-0.944120330982807,-1.96035898492369E-16,
-0.329600971820345));
#24634=DIRECTION('ref_axis',(-0.329600971820345,-6.84379104382785E-17,0.944120330982807));
#24635=DIRECTION('',(-0.329600971820918,-6.84379104383976E-17,0.944120330982607));
#24636=DIRECTION('',(2.07638679158937E-16,-1.,1.20948400507518E-31));
#24637=DIRECTION('',(0.329600971820918,6.84379104383976E-17,-0.944120330982607));
#24638=DIRECTION('center_axis',(2.07638679158937E-16,-1.,1.20948400507518E-31));
#24639=DIRECTION('ref_axis',(-0.914294914418656,-1.89842988391623E-16,0.405049144509876));
#24640=DIRECTION('center_axis',(2.07638679158937E-16,-1.,1.20948400507518E-31));
#24641=DIRECTION('ref_axis',(-0.914294914417583,-1.898429883914E-16,0.405049144512298));
#24642=DIRECTION('',(2.07638679158937E-16,-1.,1.20948400507518E-31));
#24643=DIRECTION('center_axis',(-2.07638679158937E-16,1.,-1.20948400507518E-31));
#24644=DIRECTION('ref_axis',(-0.914294914417583,-1.898429883914E-16,0.405049144512298));
#24645=DIRECTION('center_axis',(2.07638679158937E-16,-1.,1.20948400507518E-31));
#24646=DIRECTION('ref_axis',(0.00551570721125941,1.14527415997345E-18,0.999984788371283));
#24647=DIRECTION('center_axis',(-2.07638679158937E-16,1.,-1.20948400507518E-31));
#24648=DIRECTION('ref_axis',(0.00551570721125941,1.14527415997345E-18,0.999984788371283));
#24649=DIRECTION('',(2.07638679158937E-16,-1.,1.20948400507518E-31));
#24650=DIRECTION('center_axis',(2.07638679158937E-16,-1.,1.20948400507518E-31));
#24651=DIRECTION('ref_axis',(0.00551570721125941,1.14527415997345E-18,0.999984788371283));
#24652=DIRECTION('center_axis',(0.00551570721125941,1.14527415997345E-18,
0.999984788371283));
#24653=DIRECTION('ref_axis',(0.999984788371283,2.07635520636443E-16,-0.00551570721125941));
#24654=DIRECTION('',(0.999984788371283,2.07635520636443E-16,-0.00551570721125941));
#24655=DIRECTION('',(2.07638679158937E-16,-1.,1.20948400507518E-31));
#24656=DIRECTION('',(-0.999984788371283,-2.07635520636443E-16,0.00551570721125941));
#24657=DIRECTION('center_axis',(2.07638679158937E-16,-1.,1.20948400507518E-31));
#24658=DIRECTION('ref_axis',(0.00551570721125941,1.14527415997345E-18,0.999984788371283));
#24659=DIRECTION('center_axis',(2.07638679158937E-16,-1.,1.20948400507518E-31));
#24660=DIRECTION('ref_axis',(0.00551570721125941,1.14527415997345E-18,0.999984788371283));
#24661=DIRECTION('',(2.07638679158937E-16,-1.,1.20948400507518E-31));
#24662=DIRECTION('center_axis',(-2.07638679158937E-16,1.,-1.20948400507518E-31));
#24663=DIRECTION('ref_axis',(0.00551570721125941,1.14527415997345E-18,0.999984788371283));
#24664=DIRECTION('center_axis',(2.07638679158937E-16,-1.,1.20948400507518E-31));
#24665=DIRECTION('ref_axis',(-0.884935146074078,-1.83746764872143E-16,-0.465714276400081));
#24666=DIRECTION('center_axis',(2.07638679158937E-16,-1.,1.20948400507518E-31));
#24667=DIRECTION('ref_axis',(-0.884935146073463,-1.83746764872015E-16,-0.465714276401249));
#24668=DIRECTION('',(2.07638679158937E-16,-1.,1.20948400507518E-31));
#24669=DIRECTION('center_axis',(-2.07638679158937E-16,1.,-1.20948400507518E-31));
#24670=DIRECTION('ref_axis',(-0.884935146073463,-1.83746764872015E-16,-0.465714276401249));
#24671=DIRECTION('center_axis',(2.07638679158937E-16,-1.,1.20948400507518E-31));
#24672=DIRECTION('ref_axis',(-0.255336757635762,-5.30177870962154E-17,-0.966852181152867));
#24673=DIRECTION('center_axis',(2.07638679158937E-16,-1.,1.20948400507518E-31));
#24674=DIRECTION('ref_axis',(-0.25533675765802,-5.3017787100837E-17,-0.966852181146989));
#24675=DIRECTION('',(2.07638679158937E-16,-1.,1.20948400507518E-31));
#24676=DIRECTION('center_axis',(-2.07638679158937E-16,1.,-1.20948400507518E-31));
#24677=DIRECTION('ref_axis',(-0.25533675765802,-5.3017787100837E-17,-0.966852181146989));
#24678=DIRECTION('center_axis',(0.999984788371283,2.07635520636443E-16,
-0.00551570721125978));
#24679=DIRECTION('ref_axis',(2.07638679158938E-16,-1.,1.17369458351054E-31));
#24680=DIRECTION('',(-0.00551570721225976,-1.14527416018116E-18,-0.999984788371277));
#24681=DIRECTION('',(2.07638679158937E-16,-1.,1.20948400507518E-31));
#24682=DIRECTION('',(0.00551570721225976,1.14527416018116E-18,0.999984788371277));
#24683=DIRECTION('center_axis',(2.07638679158937E-16,-1.,1.20948400507518E-31));
#24684=DIRECTION('ref_axis',(-0.999984788371283,-2.07635520636442E-16,0.00551570721125905));
#24685=DIRECTION('center_axis',(-2.07638679158937E-16,1.,-1.20948400507518E-31));
#24686=DIRECTION('ref_axis',(-0.999984788371424,-2.07635520636472E-16,0.00551570718561842));
#24687=DIRECTION('',(2.07638679158937E-16,-1.,1.20948400507518E-31));
#24688=DIRECTION('center_axis',(2.07638679158937E-16,-1.,1.20948400507518E-31));
#24689=DIRECTION('ref_axis',(-0.999984788371424,-2.07635520636472E-16,0.00551570718561842));
#24690=DIRECTION('center_axis',(-0.999984788371283,-2.07635520636443E-16,
0.00551570721125904));
#24691=DIRECTION('ref_axis',(0.00551570721125904,1.14527415997337E-18,0.999984788371283));
#24692=DIRECTION('',(0.00551570721025906,1.14527415976574E-18,0.999984788371289));
#24693=DIRECTION('',(2.07638679158937E-16,-1.,1.20948400507518E-31));
#24694=DIRECTION('',(-0.00551570721025906,-1.14527415976574E-18,-0.999984788371289));
#24695=DIRECTION('center_axis',(2.07638679158937E-16,-1.,1.20948400507518E-31));
#24696=DIRECTION('ref_axis',(-0.999984788371283,-2.07635520636442E-16,0.00551570721125908));
#24697=DIRECTION('center_axis',(2.07638679158937E-16,-1.,1.20948400507518E-31));
#24698=DIRECTION('ref_axis',(-0.99998478837146,-2.07635520636479E-16,0.00551570717920828));
#24699=DIRECTION('',(2.07638679158937E-16,-1.,1.20948400507518E-31));
#24700=DIRECTION('center_axis',(-2.07638679158937E-16,1.,-1.20948400507518E-31));
#24701=DIRECTION('ref_axis',(-0.99998478837146,-2.07635520636479E-16,0.00551570717920828));
#24702=DIRECTION('center_axis',(2.07638679158937E-16,-1.,1.20948400507518E-31));
#24703=DIRECTION('ref_axis',(0.24465563654988,5.07999732220059E-17,-0.969610034758496));
#24704=DIRECTION('center_axis',(2.07638679158937E-16,-1.,1.20948400507518E-31));
#24705=DIRECTION('ref_axis',(0.244655636552112,5.07999732224693E-17,-0.969610034757934));
#24706=DIRECTION('',(2.07638679158937E-16,-1.,1.20948400507518E-31));
#24707=DIRECTION('center_axis',(-2.07638679158937E-16,1.,-1.20948400507518E-31));
#24708=DIRECTION('ref_axis',(0.244655636552112,5.07999732224693E-17,-0.969610034757934));
#24709=DIRECTION('center_axis',(2.07638679158937E-16,-1.,1.20948400507518E-31));
#24710=DIRECTION('ref_axis',(0.879743892228186,1.82668859780403E-16,-0.475447877361127));
#24711=DIRECTION('center_axis',(2.07638679158937E-16,-1.,1.20948400507518E-31));
#24712=DIRECTION('ref_axis',(0.879743892224003,1.82668859779534E-16,-0.475447877368867));
#24713=DIRECTION('',(2.07638679158937E-16,-1.,1.20948400507518E-31));
#24714=DIRECTION('center_axis',(-2.07638679158937E-16,1.,-1.20948400507518E-31));
#24715=DIRECTION('ref_axis',(0.879743892224003,1.82668859779534E-16,-0.475447877368867));
#24716=DIRECTION('center_axis',(0.00551570721125941,1.14527415997345E-18,
0.999984788371283));
#24717=DIRECTION('ref_axis',(0.999984788371283,2.07635520636443E-16,-0.00551570721125941));
#24718=DIRECTION('',(0.999984788371283,2.07635520636443E-16,-0.00551570721125941));
#24719=DIRECTION('',(2.07638679158937E-16,-1.,1.20948400507518E-31));
#24720=DIRECTION('',(-0.999984788371283,-2.07635520636443E-16,0.00551570721125941));
#24721=DIRECTION('center_axis',(2.07638679158937E-16,-1.,1.20948400507518E-31));
#24722=DIRECTION('ref_axis',(0.945378697202868,1.962971839922E-16,-0.325974107675761));
#24723=DIRECTION('center_axis',(-2.07638679158937E-16,1.,-1.20948400507518E-31));
#24724=DIRECTION('ref_axis',(0.945378697185416,1.96297183988576E-16,-0.325974107726375));
#24725=DIRECTION('',(2.07638679158937E-16,-1.,1.20948400507518E-31));
#24726=DIRECTION('center_axis',(2.07638679158937E-16,-1.,1.20948400507518E-31));
#24727=DIRECTION('ref_axis',(0.945378697185416,1.96297183988576E-16,-0.325974107726375));
#24728=DIRECTION('center_axis',(2.07638679158937E-16,-1.,1.20948400507518E-31));
#24729=DIRECTION('ref_axis',(0.945378697202867,1.962971839922E-16,-0.325974107675763));
#24730=DIRECTION('center_axis',(2.07638679158937E-16,-1.,1.20948400507518E-31));
#24731=DIRECTION('ref_axis',(0.94537869720182,1.96297183991983E-16,-0.3259741076788));
#24732=DIRECTION('',(2.07638679158937E-16,-1.,1.20948400507518E-31));
#24733=DIRECTION('center_axis',(-2.07638679158937E-16,1.,-1.20948400507518E-31));
#24734=DIRECTION('ref_axis',(0.94537869720182,1.96297183991983E-16,-0.3259741076788));
#24735=DIRECTION('center_axis',(0.94042697538271,1.952690150139E-16,-0.339995741109396));
#24736=DIRECTION('ref_axis',(-2.07638679158937E-16,1.,-1.30537451319996E-31));
#24737=DIRECTION('',(-0.339995741109967,-7.05962666037377E-17,-0.940426975382504));
#24738=DIRECTION('',(2.07638679158937E-16,-1.,1.20948400507518E-31));
#24739=DIRECTION('',(0.339995741109967,7.05962666037377E-17,0.940426975382504));
#24740=DIRECTION('center_axis',(2.07638679158937E-16,-1.,1.20948400507518E-31));
#24741=DIRECTION('ref_axis',(-0.799654090863859,-1.66039119211012E-16,-0.600460935419362));
#24742=DIRECTION('center_axis',(-2.07638679158937E-16,1.,-1.20948400507518E-31));
#24743=DIRECTION('ref_axis',(-0.799654090861894,-1.66039119210604E-16,-0.600460935421979));
#24744=DIRECTION('center_axis',(2.07638679158937E-16,-1.,1.20948400507518E-31));
#24745=DIRECTION('ref_axis',(-0.799654090861894,-1.66039119210604E-16,-0.600460935421979));
#24746=DIRECTION('center_axis',(2.07638679158937E-16,-1.,1.20948400507518E-31));
#24747=DIRECTION('ref_axis',(0.999984788371283,2.07635520636442E-16,-0.00551570721125941));
#24748=DIRECTION('center_axis',(2.07638679158937E-16,-1.,1.20948400507518E-31));
#24749=DIRECTION('ref_axis',(0.999984788371283,2.07635520636442E-16,-0.00551570721125941));
#24750=DIRECTION('axis',(0.,0.,1.));
#24751=DIRECTION('refdir',(1.,0.,0.));
#24752=DIRECTION('center_axis',(0.,-1.,0.));
#24753=DIRECTION('ref_axis',(0.877771605587211,0.,-0.479079334165908));
#24754=DIRECTION('center_axis',(0.,1.,0.));
#24755=DIRECTION('ref_axis',(0.877771605579571,0.,-0.479079334179906));
#24756=DIRECTION('',(0.,-1.,0.));
#24757=DIRECTION('center_axis',(0.,-1.,0.));
#24758=DIRECTION('ref_axis',(0.877771605579571,0.,-0.479079334179906));
#24759=DIRECTION('',(0.,1.,0.));
#24760=DIRECTION('center_axis',(0.,-1.,0.));
#24761=DIRECTION('ref_axis',(0.290991366091359,0.,-0.956725679001188));
#24762=DIRECTION('center_axis',(0.,-1.,0.));
#24763=DIRECTION('ref_axis',(0.290991366091832,0.,-0.956725679001044));
#24764=DIRECTION('',(0.,1.,0.));
#24765=DIRECTION('center_axis',(0.,1.,0.));
#24766=DIRECTION('ref_axis',(0.290991366091832,0.,-0.956725679001044));
#24767=DIRECTION('center_axis',(0.,-1.,0.));
#24768=DIRECTION('ref_axis',(-0.520632842076221,0.,-0.853780676609419));
#24769=DIRECTION('center_axis',(0.,1.,0.));
#24770=DIRECTION('ref_axis',(-0.520632842087598,0.,-0.853780676602481));
#24771=DIRECTION('',(0.,-1.,0.));
#24772=DIRECTION('center_axis',(0.,-1.,0.));
#24773=DIRECTION('ref_axis',(-0.520632842087598,0.,-0.853780676602481));
#24774=DIRECTION('center_axis',(-0.974044425513625,0.,-0.22635692418354));
#24775=DIRECTION('ref_axis',(-0.22635692418354,0.,0.974044425513625));
#24776=DIRECTION('',(0.226356924184268,0.,-0.974044425513455));
#24777=DIRECTION('',(0.,1.,0.));
#24778=DIRECTION('',(-0.226356924184268,0.,0.974044425513455));
#24779=DIRECTION('center_axis',(0.,-1.,0.));
#24780=DIRECTION('ref_axis',(0.80772974655928,0.,-0.589552929365364));
#24781=DIRECTION('center_axis',(0.,1.,0.));
#24782=DIRECTION('ref_axis',(0.807729746554134,0.,-0.589552929372413));
#24783=DIRECTION('',(0.,-1.,0.));
#24784=DIRECTION('center_axis',(0.,-1.,0.));
#24785=DIRECTION('ref_axis',(0.807729746554134,0.,-0.589552929372413));
#24786=DIRECTION('',(0.,1.,0.));
#24787=DIRECTION('center_axis',(0.,-1.,0.));
#24788=DIRECTION('ref_axis',(0.163624134736254,0.,-0.986522753174914));
#24789=DIRECTION('center_axis',(0.,-1.,0.));
#24790=DIRECTION('ref_axis',(0.163624134736857,0.,-0.986522753174814));
#24791=DIRECTION('',(0.,1.,0.));
#24792=DIRECTION('center_axis',(0.,1.,0.));
#24793=DIRECTION('ref_axis',(0.163624134736857,0.,-0.986522753174814));
#24794=DIRECTION('center_axis',(0.,-1.,0.));
#24795=DIRECTION('ref_axis',(-0.627619496647803,0.,-0.778520242143747));
#24796=DIRECTION('center_axis',(0.,1.,0.));
#24797=DIRECTION('ref_axis',(-0.627619496652502,0.,-0.778520242139959));
#24798=DIRECTION('',(0.,-1.,0.));
#24799=DIRECTION('center_axis',(0.,-1.,0.));
#24800=DIRECTION('ref_axis',(-0.627619496652502,0.,-0.778520242139959));
#24801=DIRECTION('center_axis',(-0.995256847821609,0.,-0.0972820994026906));
#24802=DIRECTION('ref_axis',(-0.0972820994026906,0.,0.995256847821609));
#24803=DIRECTION('',(0.0972820994035842,0.,-0.995256847821521));
#24804=DIRECTION('',(0.,1.,0.));
#24805=DIRECTION('',(-0.0972820994035842,0.,0.995256847821521));
#24806=DIRECTION('center_axis',(0.,-1.,0.));
#24807=DIRECTION('ref_axis',(0.723867407622732,0.,-0.689939110488415));
#24808=DIRECTION('center_axis',(0.,1.,0.));
#24809=DIRECTION('ref_axis',(0.723867407621795,0.,-0.689939110489398));
#24810=DIRECTION('',(0.,-1.,0.));
#24811=DIRECTION('center_axis',(0.,-1.,0.));
#24812=DIRECTION('ref_axis',(0.723867407621795,0.,-0.689939110489398));
#24813=DIRECTION('',(0.,1.,0.));
#24814=DIRECTION('center_axis',(0.,-1.,0.));
#24815=DIRECTION('ref_axis',(0.0334572490706318,0.,-0.999440149526036));
#24816=DIRECTION('center_axis',(0.,-1.,0.));
#24817=DIRECTION('ref_axis',(0.0334572490713496,0.,-0.999440149526012));
#24818=DIRECTION('',(0.,1.,0.));
#24819=DIRECTION('center_axis',(0.,1.,0.));
#24820=DIRECTION('ref_axis',(0.0334572490713496,0.,-0.999440149526012));
#24821=DIRECTION('center_axis',(0.,-1.,0.));
#24822=DIRECTION('ref_axis',(-0.723867407622738,0.,-0.689939110488409));
#24823=DIRECTION('center_axis',(0.,1.,0.));
#24824=DIRECTION('ref_axis',(-0.723867407621802,0.,-0.689939110489391));
#24825=DIRECTION('',(0.,-1.,0.));
#24826=DIRECTION('center_axis',(0.,-1.,0.));
#24827=DIRECTION('ref_axis',(-0.723867407621802,0.,-0.689939110489391));
#24828=DIRECTION('center_axis',(-0.999440149526036,0.,0.0334572490706321));
#24829=DIRECTION('ref_axis',(0.,1.,0.));
#24830=DIRECTION('',(-0.0334572490715975,0.,-0.999440149526004));
#24831=DIRECTION('',(0.,1.,0.));
#24832=DIRECTION('',(0.0334572490715975,0.,0.999440149526004));
#24833=DIRECTION('center_axis',(0.,-1.,0.));
#24834=DIRECTION('ref_axis',(0.627619496647802,0.,-0.778520242143748));
#24835=DIRECTION('center_axis',(0.,1.,0.));
#24836=DIRECTION('ref_axis',(0.627619496652501,0.,-0.77852024213996));
#24837=DIRECTION('',(0.,-1.,0.));
#24838=DIRECTION('center_axis',(0.,-1.,0.));
#24839=DIRECTION('ref_axis',(0.627619496652501,0.,-0.77852024213996));
#24840=DIRECTION('',(0.,1.,0.));
#24841=DIRECTION('center_axis',(0.,-1.,0.));
#24842=DIRECTION('ref_axis',(-0.097282099402691,0.,-0.995256847821609));
#24843=DIRECTION('center_axis',(0.,-1.,0.));
#24844=DIRECTION('ref_axis',(-0.0972820994033555,0.,-0.995256847821544));
#24845=DIRECTION('',(0.,1.,0.));
#24846=DIRECTION('center_axis',(0.,1.,0.));
#24847=DIRECTION('ref_axis',(-0.0972820994033555,0.,-0.995256847821544));
#24848=DIRECTION('center_axis',(0.,-1.,0.));
#24849=DIRECTION('ref_axis',(-0.807729746559285,0.,-0.589552929365357));
#24850=DIRECTION('center_axis',(0.,1.,0.));
#24851=DIRECTION('ref_axis',(-0.80772974655414,0.,-0.589552929372406));
#24852=DIRECTION('',(0.,-1.,0.));
#24853=DIRECTION('center_axis',(0.,-1.,0.));
#24854=DIRECTION('ref_axis',(-0.80772974655414,0.,-0.589552929372406));
#24855=DIRECTION('center_axis',(-0.986522753174914,0.,0.163624134736254));
#24856=DIRECTION('ref_axis',(0.,1.,0.));
#24857=DIRECTION('',(-0.163624134737066,0.,-0.986522753174779));
#24858=DIRECTION('',(0.,1.,0.));
#24859=DIRECTION('',(0.163624134737066,0.,0.986522753174779));
#24860=DIRECTION('center_axis',(0.,-1.,0.));
#24861=DIRECTION('ref_axis',(0.520632842076226,0.,-0.853780676609416));
#24862=DIRECTION('center_axis',(0.,1.,0.));
#24863=DIRECTION('ref_axis',(0.520632842087603,0.,-0.853780676602478));
#24864=DIRECTION('',(0.,-1.,0.));
#24865=DIRECTION('center_axis',(0.,-1.,0.));
#24866=DIRECTION('ref_axis',(0.520632842087603,0.,-0.853780676602478));
#24867=DIRECTION('',(0.,1.,0.));
#24868=DIRECTION('center_axis',(0.,-1.,0.));
#24869=DIRECTION('ref_axis',(-0.22635692418354,0.,-0.974044425513625));
#24870=DIRECTION('center_axis',(0.,-1.,0.));
#24871=DIRECTION('ref_axis',(-0.226356924184081,0.,-0.974044425513499));
#24872=DIRECTION('',(0.,1.,0.));
#24873=DIRECTION('center_axis',(0.,1.,0.));
#24874=DIRECTION('ref_axis',(-0.226356924184081,0.,-0.974044425513499));
#24875=DIRECTION('center_axis',(0.,-1.,0.));
#24876=DIRECTION('ref_axis',(-0.877771605587215,0.,-0.4790793341659));
#24877=DIRECTION('center_axis',(0.,1.,0.));
#24878=DIRECTION('ref_axis',(-0.877771605579575,0.,-0.479079334179899));
#24879=DIRECTION('',(0.,-1.,0.));
#24880=DIRECTION('center_axis',(0.,-1.,0.));
#24881=DIRECTION('ref_axis',(-0.877771605579575,0.,-0.479079334179899));
#24882=DIRECTION('center_axis',(-0.956725679001188,0.,0.290991366091359));
#24883=DIRECTION('ref_axis',(0.,1.,0.));
#24884=DIRECTION('',(-0.290991366091996,0.,-0.956725679000994));
#24885=DIRECTION('',(0.,1.,0.));
#24886=DIRECTION('',(0.290991366091996,0.,0.956725679000994));
#24887=DIRECTION('center_axis',(0.974044425513625,0.,-0.22635692418354));
#24888=DIRECTION('ref_axis',(0.,-1.,0.));
#24889=DIRECTION('',(-0.226356924184268,0.,-0.974044425513455));
#24890=DIRECTION('',(0.,-1.,0.));
#24891=DIRECTION('',(0.226356924184268,0.,0.974044425513455));
#24892=DIRECTION('center_axis',(0.995256847821609,0.,-0.0972820994026909));
#24893=DIRECTION('ref_axis',(0.,-1.,0.));
#24894=DIRECTION('',(-0.0972820994035846,0.,-0.995256847821521));
#24895=DIRECTION('',(0.,-1.,0.));
#24896=DIRECTION('',(0.0972820994035846,0.,0.995256847821521));
#24897=DIRECTION('center_axis',(0.986522753174914,0.,0.163624134736254));
#24898=DIRECTION('ref_axis',(0.,-1.,0.));
#24899=DIRECTION('',(0.163624134737066,0.,-0.986522753174779));
#24900=DIRECTION('',(0.,-1.,0.));
#24901=DIRECTION('',(-0.163624134737066,0.,0.986522753174779));
#24902=DIRECTION('center_axis',(0.956725679001189,0.,0.290991366091358));
#24903=DIRECTION('ref_axis',(0.,-1.,0.));
#24904=DIRECTION('',(0.290991366091995,0.,-0.956725679000995));
#24905=DIRECTION('',(0.,-1.,0.));
#24906=DIRECTION('',(-0.290991366091995,0.,0.956725679000995));
#24907=DIRECTION('center_axis',(0.,1.,0.));
#24908=DIRECTION('ref_axis',(-0.333806859233771,0.,0.942641491092178));
#24909=DIRECTION('center_axis',(0.,-1.,0.));
#24910=DIRECTION('ref_axis',(-0.333806859234212,0.,0.942641491092022));
#24911=DIRECTION('',(0.,-1.,0.));
#24912=DIRECTION('center_axis',(0.,1.,0.));
#24913=DIRECTION('ref_axis',(-0.333806859234212,0.,0.942641491092022));
#24914=DIRECTION('center_axis',(0.,1.,0.));
#24915=DIRECTION('ref_axis',(-0.333806859233771,0.,0.942641491092178));
#24916=DIRECTION('center_axis',(0.,1.,0.));
#24917=DIRECTION('ref_axis',(-0.333806859234212,0.,0.942641491092022));
#24918=DIRECTION('center_axis',(0.,-1.,0.));
#24919=DIRECTION('ref_axis',(-0.333806859234212,0.,0.942641491092022));
#24920=DIRECTION('center_axis',(0.,1.,0.));
#24921=DIRECTION('ref_axis',(1.,0.,0.));
#24922=DIRECTION('',(-0.333806859234348,0.,-0.942641491091974));
#24923=DIRECTION('center_axis',(0.,-1.,0.));
#24924=DIRECTION('ref_axis',(0.333806859234184,0.,-0.942641491092032));
#24925=DIRECTION('',(-0.333806859234344,0.,0.942641491091975));
#24926=DIRECTION('center_axis',(0.,1.,0.));
#24927=DIRECTION('ref_axis',(-0.333806859234212,0.,0.942641491092022));
#24928=DIRECTION('center_axis',(0.,1.,0.));
#24929=DIRECTION('ref_axis',(-0.333806859234212,0.,0.942641491092022));
#24930=DIRECTION('center_axis',(0.,1.,0.));
#24931=DIRECTION('ref_axis',(-0.333806859234212,0.,0.942641491092022));
#24932=DIRECTION('',(0.0334572490715973,0.,-0.999440149526004));
#24933=DIRECTION('center_axis',(0.,1.,0.));
#24934=DIRECTION('ref_axis',(-0.333806859234212,0.,0.942641491092022));
#24935=DIRECTION('center_axis',(0.,1.,0.));
#24936=DIRECTION('ref_axis',(-0.333806859233771,0.,0.942641491092178));
#24937=DIRECTION('center_axis',(0.,-1.,0.));
#24938=DIRECTION('ref_axis',(-0.333806859234212,0.,0.942641491092022));
#24939=DIRECTION('',(0.,-1.,0.));
#24940=DIRECTION('center_axis',(0.,1.,0.));
#24941=DIRECTION('ref_axis',(-0.333806859233771,0.,0.942641491092178));
#24942=DIRECTION('',(0.,1.,0.));
#24943=DIRECTION('center_axis',(0.,-1.,0.));
#24944=DIRECTION('ref_axis',(-0.333806859234212,0.,0.942641491092022));
#24945=DIRECTION('center_axis',(0.999440149526036,0.,0.0334572490706318));
#24946=DIRECTION('ref_axis',(0.,-1.,0.));
#24947=DIRECTION('',(-0.0334572490715973,0.,0.999440149526004));
#24948=DIRECTION('center_axis',(0.,1.,0.));
#24949=DIRECTION('ref_axis',(-0.333806859233771,0.,0.942641491092178));
#24950=DIRECTION('center_axis',(0.,-1.,0.));
#24951=DIRECTION('ref_axis',(-0.333806859234212,0.,0.942641491092022));
#24952=DIRECTION('center_axis',(-0.942641491092177,0.,0.333806859233774));
#24953=DIRECTION('ref_axis',(0.,1.,0.));
#24954=DIRECTION('',(0.333806859234348,0.,0.942641491091974));
#24955=DIRECTION('',(0.,1.,0.));
#24956=DIRECTION('center_axis',(0.,1.,0.));
#24957=DIRECTION('ref_axis',(0.333806859233771,0.,-0.942641491092178));
#24958=DIRECTION('center_axis',(0.,1.,0.));
#24959=DIRECTION('ref_axis',(0.333806859234184,0.,-0.942641491092032));
#24960=DIRECTION('',(0.,1.,0.));
#24961=DIRECTION('center_axis',(0.942641491092179,0.,0.33380685923377));
#24962=DIRECTION('ref_axis',(0.,-1.,0.));
#24963=DIRECTION('',(0.333806859234344,0.,-0.942641491091975));
#24964=DIRECTION('center_axis',(0.,1.,0.));
#24965=DIRECTION('ref_axis',(-0.333806859233771,0.,0.942641491092178));
#24966=DIRECTION('center_axis',(0.,-1.,0.));
#24967=DIRECTION('ref_axis',(-0.333806859234212,0.,0.942641491092022));
#24968=DIRECTION('center_axis',(0.,1.,0.));
#24969=DIRECTION('ref_axis',(1.,0.,0.));
#24970=DIRECTION('axis',(0.,0.,1.));
#24971=DIRECTION('refdir',(1.,0.,0.));
#24972=DIRECTION('center_axis',(0.,-1.,0.));
#24973=DIRECTION('ref_axis',(0.560568426942125,0.,0.828108108108858));
#24974=DIRECTION('center_axis',(0.,-1.,0.));
#24975=DIRECTION('ref_axis',(0.560568426942125,0.,0.828108108108858));
#24976=DIRECTION('',(0.,-1.,0.));
#24977=DIRECTION('center_axis',(0.,0.713250449154181,0.700909264299851));
#24978=DIRECTION('ref_axis',(9.89833838717548E-17,-0.700909264299851,0.713250449154181));
#24979=DIRECTION('center_axis',(0.,0.0174524064372833,0.999847695156391));
#24980=DIRECTION('ref_axis',(1.21100396635998E-18,-0.999847695156391,0.0174524064372833));
#24981=DIRECTION('center_axis',(0.,-1.,0.));
#24982=DIRECTION('ref_axis',(0.828108108108418,0.,0.560568426942775));
#24983=DIRECTION('center_axis',(0.,-1.,0.));
#24984=DIRECTION('ref_axis',(0.828108108108418,0.,0.560568426942775));
#24985=DIRECTION('',(0.,-1.,0.));
#24986=DIRECTION('center_axis',(0.700909264299845,0.713250449154187,0.));
#24987=DIRECTION('ref_axis',(0.713250449154187,-0.700909264299845,6.30341947044217E-17));
#24988=DIRECTION('center_axis',(0.,1.,0.));
#24989=DIRECTION('ref_axis',(0.828108108108418,0.,0.560568426942775));
#24990=DIRECTION('center_axis',(0.,0.713250449154181,0.700909264299851));
#24991=DIRECTION('ref_axis',(0.,-0.700909264299851,0.713250449154181));
#24992=DIRECTION('center_axis',(0.,-1.,0.));
#24993=DIRECTION('ref_axis',(-0.828108108108883,0.,0.560568426942087));
#24994=DIRECTION('center_axis',(0.,-1.,0.));
#24995=DIRECTION('ref_axis',(-0.828108108108883,0.,0.560568426942087));
#24996=DIRECTION('',(0.,-1.,0.));
#24997=DIRECTION('center_axis',(-0.700909264299851,0.713250449154181,0.));
#24998=DIRECTION('ref_axis',(-0.713250449154181,-0.700909264299851,0.));
#24999=DIRECTION('center_axis',(-0.999847695156391,0.0174524064372833,0.));
#25000=DIRECTION('ref_axis',(-0.0174524064372833,-0.999847695156391,0.));
#25001=DIRECTION('center_axis',(0.,-1.,0.));
#25002=DIRECTION('ref_axis',(-0.560568426943144,0.,0.828108108108168));
#25003=DIRECTION('center_axis',(0.,-1.,0.));
#25004=DIRECTION('ref_axis',(-0.560568426943144,0.,0.828108108108168));
#25005=DIRECTION('',(0.,-1.,0.));
#25006=DIRECTION('center_axis',(0.,0.713250449154181,0.700909264299851));
#25007=DIRECTION('ref_axis',(6.30341947044626E-17,-0.700909264299851,0.713250449154181));
#25008=DIRECTION('center_axis',(0.,1.,0.));
#25009=DIRECTION('ref_axis',(-0.560568426943144,0.,0.828108108108168));
#25010=DIRECTION('center_axis',(-0.700909264299851,0.713250449154181,0.));
#25011=DIRECTION('ref_axis',(-0.713250449154181,-0.700909264299851,6.30341947044626E-17));
#25012=DIRECTION('center_axis',(0.,-1.,0.));
#25013=DIRECTION('ref_axis',(-0.560568426942121,0.,-0.82810810810886));
#25014=DIRECTION('center_axis',(0.,-1.,0.));
#25015=DIRECTION('ref_axis',(-0.560568426942121,0.,-0.82810810810886));
#25016=DIRECTION('',(0.,-1.,0.));
#25017=DIRECTION('center_axis',(0.,0.713250449154181,-0.700909264299851));
#25018=DIRECTION('ref_axis',(0.,-0.700909264299851,-0.713250449154181));
#25019=DIRECTION('center_axis',(0.,0.0174524064372833,-0.999847695156391));
#25020=DIRECTION('ref_axis',(0.,-0.999847695156391,-0.0174524064372833));
#25021=DIRECTION('center_axis',(0.,-1.,0.));
#25022=DIRECTION('ref_axis',(-0.828108108107798,0.,-0.56056842694369));
#25023=DIRECTION('center_axis',(0.,-1.,0.));
#25024=DIRECTION('ref_axis',(-0.828108108107798,0.,-0.56056842694369));
#25025=DIRECTION('',(0.,-1.,0.));
#25026=DIRECTION('center_axis',(-0.700909264299851,0.713250449154181,0.));
#25027=DIRECTION('ref_axis',(-0.713250449154181,-0.700909264299851,-1.26068389408919E-16));
#25028=DIRECTION('center_axis',(0.,1.,0.));
#25029=DIRECTION('ref_axis',(-0.828108108107798,0.,-0.56056842694369));
#25030=DIRECTION('center_axis',(0.,0.713250449154181,-0.700909264299851));
#25031=DIRECTION('ref_axis',(6.30341947044594E-17,-0.700909264299851,-0.713250449154181));
#25032=DIRECTION('center_axis',(0.,-1.,0.));
#25033=DIRECTION('ref_axis',(0.828108108108829,0.,-0.560568426942167));
#25034=DIRECTION('center_axis',(0.,-1.,0.));
#25035=DIRECTION('ref_axis',(0.828108108108829,0.,-0.560568426942167));
#25036=DIRECTION('',(0.,-1.,0.));
#25037=DIRECTION('center_axis',(0.700909264299845,0.713250449154187,0.));
#25038=DIRECTION('ref_axis',(0.713250449154187,-0.700909264299845,1.48475075808888E-16));
#25039=DIRECTION('center_axis',(0.999847695156391,0.0174524064372833,0.));
#25040=DIRECTION('ref_axis',(0.0174524064372833,-0.999847695156391,0.));
#25041=DIRECTION('center_axis',(0.,-1.,0.));
#25042=DIRECTION('ref_axis',(0.560568426943322,0.,-0.828108108108047));
#25043=DIRECTION('center_axis',(0.,-1.,0.));
#25044=DIRECTION('ref_axis',(0.560568426943322,0.,-0.828108108108047));
#25045=DIRECTION('',(0.,-1.,0.));
#25046=DIRECTION('center_axis',(0.,0.713250449154181,-0.700909264299851));
#25047=DIRECTION('ref_axis',(1.26068389408919E-16,-0.700909264299851,-0.713250449154181));
#25048=DIRECTION('center_axis',(0.,1.,0.));
#25049=DIRECTION('ref_axis',(0.560568426943322,0.,-0.828108108108047));
#25050=DIRECTION('center_axis',(0.700909264299845,0.713250449154187,0.));
#25051=DIRECTION('ref_axis',(0.713250449154187,-0.700909264299845,0.));
#25052=DIRECTION('center_axis',(0.,-1.,0.));
#25053=DIRECTION('ref_axis',(1.,0.,-5.00979119302536E-12));
#25054=DIRECTION('center_axis',(0.,-1.,0.));
#25055=DIRECTION('ref_axis',(1.,0.,-5.00979119302536E-12));
#25056=DIRECTION('center_axis',(0.999847695156391,0.0174524064372833,0.));
#25057=DIRECTION('ref_axis',(0.0174524064372833,-0.999847695156391,-8.74329120666009E-14));
#25058=DIRECTION('center_axis',(0.700909264299845,0.713250449154187,0.));
#25059=DIRECTION('ref_axis',(0.713250449154187,-0.700909264299845,-3.57323581859403E-12));
#25060=DIRECTION('center_axis',(0.,-1.,0.));
#25061=DIRECTION('ref_axis',(5.06308189820828E-12,0.,1.));
#25062=DIRECTION('center_axis',(0.,-1.,0.));
#25063=DIRECTION('ref_axis',(5.06308189820828E-12,0.,1.));
#25064=DIRECTION('center_axis',(0.,0.0174524064372833,0.999847695156391));
#25065=DIRECTION('ref_axis',(8.83629631127828E-14,-0.999847695156391,0.0174524064372833));
#25066=DIRECTION('center_axis',(0.,0.713250449154181,0.700909264299851));
#25067=DIRECTION('ref_axis',(3.61124543800146E-12,-0.700909264299851,0.713250449154181));
#25068=DIRECTION('center_axis',(0.,-1.,0.));
#25069=DIRECTION('ref_axis',(-1.,0.,5.0097911930254E-12));
#25070=DIRECTION('center_axis',(0.,-1.,0.));
#25071=DIRECTION('ref_axis',(-1.,0.,5.0097911930254E-12));
#25072=DIRECTION('center_axis',(-0.999847695156391,0.0174524064372833,0.));
#25073=DIRECTION('ref_axis',(-0.0174524064372833,-0.999847695156391,8.74329120666017E-14));
#25074=DIRECTION('center_axis',(-0.700909264299851,0.713250449154181,0.));
#25075=DIRECTION('ref_axis',(-0.713250449154181,-0.700909264299851,3.57323581859403E-12));
#25076=DIRECTION('center_axis',(0.,-1.,0.));
#25077=DIRECTION('ref_axis',(-4.92541424309684E-12,0.,-1.));
#25078=DIRECTION('center_axis',(0.,-1.,0.));
#25079=DIRECTION('ref_axis',(-4.92541424309684E-12,0.,-1.));
#25080=DIRECTION('center_axis',(0.,0.0174524064372833,-0.999847695156391));
#25081=DIRECTION('ref_axis',(-8.59603312425102E-14,-0.999847695156391,-0.0174524064372833));
#25082=DIRECTION('center_axis',(0.,0.713250449154181,-0.700909264299851));
#25083=DIRECTION('ref_axis',(-3.51305392115922E-12,-0.700909264299851,-0.713250449154181));
#25084=DIRECTION('center_axis',(0.,0.0174524064372833,0.999847695156391));
#25085=DIRECTION('ref_axis',(1.,0.,0.));
#25086=DIRECTION('',(1.,0.,0.));
#25087=DIRECTION('',(1.,0.,0.));
#25088=DIRECTION('center_axis',(0.,0.713250449154181,0.700909264299851));
#25089=DIRECTION('ref_axis',(1.,0.,0.));
#25090=DIRECTION('',(-1.,0.,0.));
#25091=DIRECTION('center_axis',(-0.999847695156391,0.0174524064372833,0.));
#25092=DIRECTION('ref_axis',(0.,0.,1.));
#25093=DIRECTION('',(0.,0.,1.));
#25094=DIRECTION('',(0.,0.,1.));
#25095=DIRECTION('center_axis',(-0.700909264299851,0.713250449154181,0.));
#25096=DIRECTION('ref_axis',(0.,0.,1.));
#25097=DIRECTION('',(0.,0.,-1.));
#25098=DIRECTION('center_axis',(0.,0.0174524064372833,-0.999847695156391));
#25099=DIRECTION('ref_axis',(-1.,0.,0.));
#25100=DIRECTION('',(-1.,0.,0.));
#25101=DIRECTION('',(-1.,0.,0.));
#25102=DIRECTION('center_axis',(0.,1.,0.));
#25103=DIRECTION('ref_axis',(1.,0.,0.));
#25104=DIRECTION('',(0.,0.,-1.));
#25105=DIRECTION('',(0.707106781186548,0.,-0.707106781186548));
#25106=DIRECTION('',(-1.00027490415113E-12,0.,-1.));
#25107=DIRECTION('',(-0.707106781186548,0.,-0.707106781186547));
#25108=DIRECTION('',(-1.,0.,1.00013745207507E-12));
#25109=DIRECTION('',(-0.707106781186547,0.,0.707106781186548));
#25110=DIRECTION('',(1.00013745207507E-12,0.,1.));
#25111=DIRECTION('',(0.707106781186548,0.,0.707106781186548));
#25112=DIRECTION('',(1.,0.,0.));
#25113=DIRECTION('center_axis',(0.,1.,0.));
#25114=DIRECTION('ref_axis',(1.,0.,0.));
#25115=DIRECTION('center_axis',(0.,1.,0.));
#25116=DIRECTION('ref_axis',(1.,0.,0.));
#25117=DIRECTION('center_axis',(0.,1.,0.));
#25118=DIRECTION('ref_axis',(1.,0.,0.));
#25119=DIRECTION('center_axis',(0.,1.,0.));
#25120=DIRECTION('ref_axis',(1.,0.,0.));
#25121=DIRECTION('center_axis',(0.,0.713250449154181,-0.700909264299851));
#25122=DIRECTION('ref_axis',(-1.,0.,0.));
#25123=DIRECTION('',(1.,0.,0.));
#25124=DIRECTION('center_axis',(0.,1.,0.));
#25125=DIRECTION('ref_axis',(1.,0.,0.));
#25126=DIRECTION('',(0.,0.,1.));
#25127=DIRECTION('center_axis',(0.,-1.,0.));
#25128=DIRECTION('ref_axis',(1.,0.,0.));
#25129=DIRECTION('center_axis',(0.,-1.,0.));
#25130=DIRECTION('ref_axis',(1.,0.,0.));
#25131=DIRECTION('center_axis',(0.,-1.,0.));
#25132=DIRECTION('ref_axis',(1.,0.,0.));
#25133=DIRECTION('center_axis',(0.,-1.,0.));
#25134=DIRECTION('ref_axis',(1.,0.,0.));
#25135=DIRECTION('center_axis',(0.,-1.,0.));
#25136=DIRECTION('ref_axis',(1.,0.,0.));
#25137=DIRECTION('center_axis',(-0.707106781186547,-0.707106781186548,1.94386590150466E-16));
#25138=DIRECTION('ref_axis',(-0.707106781186548,0.707106781186547,3.74194010293243E-33));
#25139=DIRECTION('',(-1.00027490415113E-12,0.,-1.));
#25140=DIRECTION('',(0.678598344545735,-0.678598344545736,-0.281084637715359));
#25141=DIRECTION('',(1.00027490415113E-12,0.,1.));
#25142=DIRECTION('',(0.678598344545735,-0.678598344545735,0.281084637715361));
#25143=DIRECTION('center_axis',(-0.500000000000001,-0.707106781186547,0.500000000000001));
#25144=DIRECTION('ref_axis',(-0.816496580927725,0.577350269189627,2.5034978194734E-16));
#25145=DIRECTION('',(-0.707106781186548,0.,-0.707106781186547));
#25146=DIRECTION('',(0.281084637715357,-0.678598344545735,-0.678598344545737));
#25147=DIRECTION('',(0.707106781186548,0.,0.707106781186547));
#25148=DIRECTION('center_axis',(9.71932950752329E-17,-0.707106781186548,
0.707106781186547));
#25149=DIRECTION('ref_axis',(-1.,-1.37452076067124E-16,2.07747144876332E-31));
#25150=DIRECTION('',(-1.,0.,1.00013745207507E-12));
#25151=DIRECTION('',(-0.281084637715359,-0.678598344545735,-0.678598344545736));
#25152=DIRECTION('',(1.,0.,-1.00013745207507E-12));
#25153=DIRECTION('center_axis',(0.5,-0.707106781186547,0.5));
#25154=DIRECTION('ref_axis',(1.18404905982997E-16,-0.577350269189626,-0.816496580927726));
#25155=DIRECTION('',(0.707106781186547,0.,-0.707106781186548));
#25156=DIRECTION('',(-0.707106781186547,0.,0.707106781186548));
#25157=DIRECTION('',(-0.678598344545736,-0.678598344545735,-0.281084637715358));
#25158=DIRECTION('center_axis',(0.707106781186547,-0.707106781186548,-9.71932950752329E-17));
#25159=DIRECTION('ref_axis',(-2.09730162168143E-31,1.37452076067124E-16,
-1.));
#25160=DIRECTION('',(-1.00013745207507E-12,0.,-1.));
#25161=DIRECTION('',(1.00013745207507E-12,0.,1.));
#25162=DIRECTION('',(-0.678598344545735,-0.678598344545735,0.28108463771536));
#25163=DIRECTION('center_axis',(0.5,-0.707106781186548,-0.5));
#25164=DIRECTION('ref_axis',(-1.2120878851009E-16,0.577350269189625,-0.816496580927726));
#25165=DIRECTION('',(-0.707106781186548,0.,-0.707106781186548));
#25166=DIRECTION('',(0.707106781186548,0.,0.707106781186548));
#25167=DIRECTION('',(-0.281084637715359,-0.678598344545735,0.678598344545736));
#25168=DIRECTION('center_axis',(0.,-0.707106781186548,-0.707106781186547));
#25169=DIRECTION('ref_axis',(0.,0.707106781186547,-0.707106781186548));
#25170=DIRECTION('',(-1.,0.,0.));
#25171=DIRECTION('',(1.,0.,0.));
#25172=DIRECTION('',(0.281084637715361,-0.678598344545735,0.678598344545735));
#25173=DIRECTION('center_axis',(-0.5,-0.707106781186548,-0.5));
#25174=DIRECTION('ref_axis',(1.2120878851009E-16,0.577350269189625,-0.816496580927726));
#25175=DIRECTION('',(-0.707106781186548,0.,0.707106781186548));
#25176=DIRECTION('',(0.707106781186548,0.,-0.707106781186548));
#25177=DIRECTION('center_axis',(-0.707106781186548,0.,0.707106781186548));
#25178=DIRECTION('ref_axis',(0.,1.,0.));
#25179=DIRECTION('',(0.,1.,0.));
#25180=DIRECTION('',(0.,1.,0.));
#25181=DIRECTION('center_axis',(0.,0.,1.));
#25182=DIRECTION('ref_axis',(1.,0.,0.));
#25183=DIRECTION('',(0.,1.,0.));
#25184=DIRECTION('center_axis',(0.707106781186548,0.,0.707106781186548));
#25185=DIRECTION('ref_axis',(0.,-1.,0.));
#25186=DIRECTION('',(0.,1.,0.));
#25187=DIRECTION('center_axis',(1.,0.,-2.74904152134249E-16));
#25188=DIRECTION('ref_axis',(0.,1.,0.));
#25189=DIRECTION('',(0.,1.,0.));
#25190=DIRECTION('center_axis',(0.,-1.,0.));
#25191=DIRECTION('ref_axis',(0.,0.,-1.));
#25192=DIRECTION('center_axis',(0.,-1.,0.));
#25193=DIRECTION('ref_axis',(-1.,0.,0.));
#25194=DIRECTION('center_axis',(0.700909264299845,0.713250449154187,0.));
#25195=DIRECTION('ref_axis',(0.,0.,-1.));
#25196=DIRECTION('',(0.,0.,-1.));
#25197=DIRECTION('center_axis',(0.,-1.,0.));
#25198=DIRECTION('ref_axis',(-1.,0.,0.));
#25199=DIRECTION('center_axis',(0.,1.,0.));
#25200=DIRECTION('ref_axis',(-1.,0.,0.));
#25201=DIRECTION('',(-0.707106781186547,0.707106781186548,-8.65956056235492E-17));
#25202=DIRECTION('center_axis',(0.,-1.,0.));
#25203=DIRECTION('ref_axis',(-1.,0.,0.));
#25204=DIRECTION('center_axis',(0.,1.,0.));
#25205=DIRECTION('ref_axis',(-1.,0.,0.));
#25206=DIRECTION('center_axis',(0.,1.,0.));
#25207=DIRECTION('ref_axis',(1.,0.,0.));
#25208=DIRECTION('center_axis',(0.,1.,0.));
#25209=DIRECTION('ref_axis',(-1.,0.,0.));
#25210=DIRECTION('center_axis',(0.,1.,0.));
#25211=DIRECTION('ref_axis',(1.,0.,0.));
#25212=DIRECTION('',(0.,-1.,0.));
#25213=DIRECTION('center_axis',(0.,1.,0.));
#25214=DIRECTION('ref_axis',(-1.,0.,0.));
#25215=DIRECTION('center_axis',(0.,-1.,0.));
#25216=DIRECTION('ref_axis',(-1.,0.,0.));
#25217=DIRECTION('',(0.707106781186545,0.70710678118655,-8.6595605623549E-17));
#25218=DIRECTION('center_axis',(0.,-1.,0.));
#25219=DIRECTION('ref_axis',(-1.,0.,0.));
#25220=DIRECTION('center_axis',(0.,1.,0.));
#25221=DIRECTION('ref_axis',(1.,0.,0.));
#25222=DIRECTION('center_axis',(0.,1.,0.));
#25223=DIRECTION('ref_axis',(1.,0.,0.));
#25224=DIRECTION('',(0.,1.,0.));
#25225=DIRECTION('center_axis',(0.,-1.,0.));
#25226=DIRECTION('ref_axis',(1.,0.,0.));
#25227=DIRECTION('',(-0.707106781186544,-0.707106781186551,-8.65956056235488E-17));
#25228=DIRECTION('center_axis',(0.,-1.,0.));
#25229=DIRECTION('ref_axis',(1.,0.,0.));
#25230=DIRECTION('center_axis',(0.,-1.,0.));
#25231=DIRECTION('ref_axis',(0.,0.,-1.));
#25232=DIRECTION('center_axis',(0.,1.,0.));
#25233=DIRECTION('ref_axis',(1.,0.,0.));
#25234=DIRECTION('center_axis',(0.,1.,0.));
#25235=DIRECTION('ref_axis',(-1.,0.,0.));
#25236=DIRECTION('center_axis',(0.,-1.,0.));
#25237=DIRECTION('ref_axis',(-1.,0.,0.));
#25238=DIRECTION('',(-0.707106781186546,-0.707106781186549,8.65956056235491E-17));
#25239=DIRECTION('center_axis',(0.,1.,0.));
#25240=DIRECTION('ref_axis',(-1.,0.,0.));
#25241=DIRECTION('center_axis',(0.,-1.,0.));
#25242=DIRECTION('ref_axis',(0.,0.,-1.));
#25243=DIRECTION('center_axis',(0.,-1.,0.));
#25244=DIRECTION('ref_axis',(-1.,0.,0.));
#25245=DIRECTION('center_axis',(0.,1.,0.));
#25246=DIRECTION('ref_axis',(-1.,0.,0.));
#25247=DIRECTION('',(0.,-1.,0.));
#25248=DIRECTION('center_axis',(0.,-1.,0.));
#25249=DIRECTION('ref_axis',(-1.,0.,0.));
#25250=DIRECTION('center_axis',(0.,1.,0.));
#25251=DIRECTION('ref_axis',(-1.,0.,0.));
#25252=DIRECTION('',(0.242535625036333,-0.970142500145332,2.97020476879948E-17));
#25253=DIRECTION('center_axis',(0.,1.,0.));
#25254=DIRECTION('ref_axis',(-1.,0.,0.));
#25255=DIRECTION('center_axis',(0.,1.,0.));
#25256=DIRECTION('ref_axis',(1.,0.,0.));
#25257=DIRECTION('',(0.,1.,0.));
#25258=DIRECTION('center_axis',(0.,1.,0.));
#25259=DIRECTION('ref_axis',(1.,0.,0.));
#25260=DIRECTION('center_axis',(0.,1.,0.));
#25261=DIRECTION('ref_axis',(1.,0.,0.));
#25262=DIRECTION('',(0.,1.,0.));
#25263=DIRECTION('center_axis',(0.,1.,0.));
#25264=DIRECTION('ref_axis',(1.,0.,0.));
#25265=DIRECTION('',(0.,1.,0.));
#25266=DIRECTION('center_axis',(0.,1.,0.));
#25267=DIRECTION('ref_axis',(1.,0.,0.));
#25268=DIRECTION('',(0.,1.,0.));
#25269=DIRECTION('center_axis',(0.,1.,0.));
#25270=DIRECTION('ref_axis',(1.,0.,0.));
#25271=DIRECTION('',(0.,1.,0.));
#25272=DIRECTION('center_axis',(0.,1.,0.));
#25273=DIRECTION('ref_axis',(1.,0.,0.));
#25274=DIRECTION('center_axis',(0.,1.,0.));
#25275=DIRECTION('ref_axis',(1.,0.,0.));
#25276=DIRECTION('',(0.,1.,0.));
#25277=DIRECTION('center_axis',(0.,-1.,0.));
#25278=DIRECTION('ref_axis',(0.,0.,-1.));
#25279=DIRECTION('center_axis',(-1.,0.,1.37452076067125E-16));
#25280=DIRECTION('ref_axis',(0.,1.,0.));
#25281=DIRECTION('',(0.,1.,0.));
#25282=DIRECTION('center_axis',(-0.707106781186548,0.,-0.707106781186547));
#25283=DIRECTION('ref_axis',(-0.707106781186547,0.,0.707106781186548));
#25284=DIRECTION('',(0.,1.,0.));
#25285=DIRECTION('center_axis',(-1.37452076067125E-16,0.,-1.));
#25286=DIRECTION('ref_axis',(-1.,0.,1.37452076067125E-16));
#25287=DIRECTION('',(0.,1.,0.));
#25288=DIRECTION('center_axis',(0.707106781186547,0.,-0.707106781186548));
#25289=DIRECTION('ref_axis',(0.,-1.,0.));
#25290=DIRECTION('center_axis',(0.999847695156391,0.0174524064372833,0.));
#25291=DIRECTION('ref_axis',(0.,0.,-1.));
#25292=DIRECTION('axis',(0.,0.,1.));
#25293=DIRECTION('refdir',(1.,0.,0.));
#25294=DIRECTION('center_axis',(0.,-1.,0.));
#25295=DIRECTION('ref_axis',(-0.479079334165917,0.,-0.877771605587206));
#25296=DIRECTION('center_axis',(0.,1.,0.));
#25297=DIRECTION('ref_axis',(-0.479079334179915,0.,-0.877771605579566));
#25298=DIRECTION('',(0.,-1.,0.));
#25299=DIRECTION('center_axis',(0.,-1.,0.));
#25300=DIRECTION('ref_axis',(-0.479079334179915,0.,-0.877771605579566));
#25301=DIRECTION('',(0.,1.,0.));
#25302=DIRECTION('center_axis',(0.,-1.,0.));
#25303=DIRECTION('ref_axis',(-0.956725679001189,0.,-0.290991366091358));
#25304=DIRECTION('center_axis',(0.,-1.,0.));
#25305=DIRECTION('ref_axis',(-0.956725679001045,0.,-0.290991366091831));
#25306=DIRECTION('',(0.,1.,0.));
#25307=DIRECTION('center_axis',(0.,1.,0.));
#25308=DIRECTION('ref_axis',(-0.956725679001045,0.,-0.290991366091831));
#25309=DIRECTION('center_axis',(0.,-1.,0.));
#25310=DIRECTION('ref_axis',(-0.853780676609416,0.,0.520632842076226));
#25311=DIRECTION('center_axis',(0.,1.,0.));
#25312=DIRECTION('ref_axis',(-0.853780676602478,0.,0.520632842087603));
#25313=DIRECTION('',(0.,-1.,0.));
#25314=DIRECTION('center_axis',(0.,-1.,0.));
#25315=DIRECTION('ref_axis',(-0.853780676602478,0.,0.520632842087603));
#25316=DIRECTION('center_axis',(-0.22635692418354,0.,0.974044425513625));
#25317=DIRECTION('ref_axis',(0.,1.,0.));
#25318=DIRECTION('',(-0.974044425513455,0.,-0.226356924184268));
#25319=DIRECTION('',(0.,1.,0.));
#25320=DIRECTION('',(0.974044425513455,0.,0.226356924184268));
#25321=DIRECTION('center_axis',(0.,-1.,0.));
#25322=DIRECTION('ref_axis',(-0.589552929365357,0.,-0.807729746559285));
#25323=DIRECTION('center_axis',(0.,1.,0.));
#25324=DIRECTION('ref_axis',(-0.589552929372406,0.,-0.80772974655414));
#25325=DIRECTION('',(0.,-1.,0.));
#25326=DIRECTION('center_axis',(0.,-1.,0.));
#25327=DIRECTION('ref_axis',(-0.589552929372406,0.,-0.80772974655414));
#25328=DIRECTION('',(0.,1.,0.));
#25329=DIRECTION('center_axis',(0.,-1.,0.));
#25330=DIRECTION('ref_axis',(-0.986522753174914,0.,-0.163624134736254));
#25331=DIRECTION('center_axis',(0.,-1.,0.));
#25332=DIRECTION('ref_axis',(-0.986522753174814,0.,-0.163624134736857));
#25333=DIRECTION('',(0.,1.,0.));
#25334=DIRECTION('center_axis',(0.,1.,0.));
#25335=DIRECTION('ref_axis',(-0.986522753174814,0.,-0.163624134736857));
#25336=DIRECTION('center_axis',(0.,-1.,0.));
#25337=DIRECTION('ref_axis',(-0.778520242143747,0.,0.627619496647803));
#25338=DIRECTION('center_axis',(0.,1.,0.));
#25339=DIRECTION('ref_axis',(-0.778520242139959,0.,0.627619496652502));
#25340=DIRECTION('',(0.,-1.,0.));
#25341=DIRECTION('center_axis',(0.,-1.,0.));
#25342=DIRECTION('ref_axis',(-0.778520242139959,0.,0.627619496652502));
#25343=DIRECTION('center_axis',(-0.0972820994026906,0.,0.995256847821609));
#25344=DIRECTION('ref_axis',(0.,1.,0.));
#25345=DIRECTION('',(-0.995256847821522,0.,-0.0972820994035843));
#25346=DIRECTION('',(0.,1.,0.));
#25347=DIRECTION('',(0.995256847821522,0.,0.0972820994035843));
#25348=DIRECTION('center_axis',(0.,-1.,0.));
#25349=DIRECTION('ref_axis',(-0.689939110488408,0.,-0.723867407622739));
#25350=DIRECTION('center_axis',(0.,1.,0.));
#25351=DIRECTION('ref_axis',(-0.689939110489391,0.,-0.723867407621802));
#25352=DIRECTION('',(0.,-1.,0.));
#25353=DIRECTION('center_axis',(0.,-1.,0.));
#25354=DIRECTION('ref_axis',(-0.689939110489391,0.,-0.723867407621802));
#25355=DIRECTION('',(0.,1.,0.));
#25356=DIRECTION('center_axis',(0.,-1.,0.));
#25357=DIRECTION('ref_axis',(-0.999440149526036,0.,-0.0334572490706319));
#25358=DIRECTION('center_axis',(0.,-1.,0.));
#25359=DIRECTION('ref_axis',(-0.999440149526012,0.,-0.0334572490713497));
#25360=DIRECTION('',(0.,1.,0.));
#25361=DIRECTION('center_axis',(0.,1.,0.));
#25362=DIRECTION('ref_axis',(-0.999440149526012,0.,-0.0334572490713497));
#25363=DIRECTION('center_axis',(0.,-1.,0.));
#25364=DIRECTION('ref_axis',(-0.689939110488409,0.,0.723867407622738));
#25365=DIRECTION('center_axis',(0.,1.,0.));
#25366=DIRECTION('ref_axis',(-0.689939110489391,0.,0.723867407621802));
#25367=DIRECTION('',(0.,-1.,0.));
#25368=DIRECTION('center_axis',(0.,-1.,0.));
#25369=DIRECTION('ref_axis',(-0.689939110489391,0.,0.723867407621802));
#25370=DIRECTION('center_axis',(0.0334572490706321,0.,0.999440149526036));
#25371=DIRECTION('ref_axis',(0.,-1.,0.));
#25372=DIRECTION('',(-0.999440149526004,0.,0.0334572490715975));
#25373=DIRECTION('',(0.,1.,0.));
#25374=DIRECTION('',(0.999440149526004,0.,-0.0334572490715975));
#25375=DIRECTION('center_axis',(0.,-1.,0.));
#25376=DIRECTION('ref_axis',(-0.778520242143747,0.,-0.627619496647803));
#25377=DIRECTION('center_axis',(0.,1.,0.));
#25378=DIRECTION('ref_axis',(-0.778520242139959,0.,-0.627619496652502));
#25379=DIRECTION('',(0.,-1.,0.));
#25380=DIRECTION('center_axis',(0.,-1.,0.));
#25381=DIRECTION('ref_axis',(-0.778520242139959,0.,-0.627619496652502));
#25382=DIRECTION('',(0.,1.,0.));
#25383=DIRECTION('center_axis',(0.,-1.,0.));
#25384=DIRECTION('ref_axis',(-0.995256847821609,0.,0.097282099402691));
#25385=DIRECTION('center_axis',(0.,-1.,0.));
#25386=DIRECTION('ref_axis',(-0.995256847821544,0.,0.0972820994033555));
#25387=DIRECTION('',(0.,1.,0.));
#25388=DIRECTION('center_axis',(0.,1.,0.));
#25389=DIRECTION('ref_axis',(-0.995256847821544,0.,0.0972820994033555));
#25390=DIRECTION('center_axis',(0.,-1.,0.));
#25391=DIRECTION('ref_axis',(-0.589552929365356,0.,0.807729746559286));
#25392=DIRECTION('center_axis',(0.,1.,0.));
#25393=DIRECTION('ref_axis',(-0.589552929372405,0.,0.807729746554141));
#25394=DIRECTION('',(0.,-1.,0.));
#25395=DIRECTION('center_axis',(0.,-1.,0.));
#25396=DIRECTION('ref_axis',(-0.589552929372405,0.,0.807729746554141));
#25397=DIRECTION('center_axis',(0.163624134736254,0.,0.986522753174914));
#25398=DIRECTION('ref_axis',(0.,-1.,0.));
#25399=DIRECTION('',(-0.986522753174779,0.,0.163624134737066));
#25400=DIRECTION('',(0.,1.,0.));
#25401=DIRECTION('',(0.986522753174779,0.,-0.163624134737066));
#25402=DIRECTION('center_axis',(0.,-1.,0.));
#25403=DIRECTION('ref_axis',(-0.853780676609419,0.,-0.520632842076221));
#25404=DIRECTION('center_axis',(0.,1.,0.));
#25405=DIRECTION('ref_axis',(-0.853780676602481,0.,-0.520632842087598));
#25406=DIRECTION('',(0.,-1.,0.));
#25407=DIRECTION('center_axis',(0.,-1.,0.));
#25408=DIRECTION('ref_axis',(-0.853780676602481,0.,-0.520632842087598));
#25409=DIRECTION('',(0.,1.,0.));
#25410=DIRECTION('center_axis',(0.,-1.,0.));
#25411=DIRECTION('ref_axis',(-0.974044425513625,0.,0.22635692418354));
#25412=DIRECTION('center_axis',(0.,-1.,0.));
#25413=DIRECTION('ref_axis',(-0.974044425513499,0.,0.226356924184081));
#25414=DIRECTION('',(0.,1.,0.));
#25415=DIRECTION('center_axis',(0.,1.,0.));
#25416=DIRECTION('ref_axis',(-0.974044425513499,0.,0.226356924184081));
#25417=DIRECTION('center_axis',(0.,-1.,0.));
#25418=DIRECTION('ref_axis',(-0.479079334165918,0.,0.877771605587206));
#25419=DIRECTION('center_axis',(0.,1.,0.));
#25420=DIRECTION('ref_axis',(-0.479079334179917,0.,0.877771605579565));
#25421=DIRECTION('',(0.,-1.,0.));
#25422=DIRECTION('center_axis',(0.,-1.,0.));
#25423=DIRECTION('ref_axis',(-0.479079334179917,0.,0.877771605579565));
#25424=DIRECTION('center_axis',(0.290991366091359,0.,0.956725679001188));
#25425=DIRECTION('ref_axis',(0.,-1.,0.));
#25426=DIRECTION('',(-0.956725679000994,0.,0.290991366091996));
#25427=DIRECTION('',(0.,1.,0.));
#25428=DIRECTION('',(0.956725679000994,0.,-0.290991366091996));
#25429=DIRECTION('center_axis',(-0.22635692418354,0.,-0.974044425513625));
#25430=DIRECTION('ref_axis',(-0.974044425513625,0.,0.22635692418354));
#25431=DIRECTION('',(-0.974044425513455,0.,0.226356924184268));
#25432=DIRECTION('',(0.,-1.,0.));
#25433=DIRECTION('',(0.974044425513455,0.,-0.226356924184268));
#25434=DIRECTION('center_axis',(-0.0972820994026909,0.,-0.995256847821609));
#25435=DIRECTION('ref_axis',(-0.995256847821609,0.,0.0972820994026909));
#25436=DIRECTION('',(-0.995256847821521,0.,0.0972820994035846));
#25437=DIRECTION('',(0.,-1.,0.));
#25438=DIRECTION('',(0.995256847821521,0.,-0.0972820994035846));
#25439=DIRECTION('center_axis',(0.163624134736254,0.,-0.986522753174914));
#25440=DIRECTION('ref_axis',(0.,-1.,0.));
#25441=DIRECTION('',(-0.986522753174779,0.,-0.163624134737066));
#25442=DIRECTION('',(0.,-1.,0.));
#25443=DIRECTION('',(0.986522753174779,0.,0.163624134737066));
#25444=DIRECTION('center_axis',(0.290991366091358,0.,-0.956725679001189));
#25445=DIRECTION('ref_axis',(0.,-1.,0.));
#25446=DIRECTION('',(-0.956725679000995,0.,-0.290991366091995));
#25447=DIRECTION('',(0.,-1.,0.));
#25448=DIRECTION('',(0.956725679000995,0.,0.290991366091995));
#25449=DIRECTION('center_axis',(0.,1.,0.));
#25450=DIRECTION('ref_axis',(0.942641491092178,0.,0.333806859233771));
#25451=DIRECTION('center_axis',(0.,-1.,0.));
#25452=DIRECTION('ref_axis',(0.942641491092022,0.,0.333806859234212));
#25453=DIRECTION('',(0.,-1.,0.));
#25454=DIRECTION('center_axis',(0.,1.,0.));
#25455=DIRECTION('ref_axis',(0.942641491092022,0.,0.333806859234212));
#25456=DIRECTION('center_axis',(0.,1.,0.));
#25457=DIRECTION('ref_axis',(0.942641491092178,0.,0.333806859233771));
#25458=DIRECTION('center_axis',(0.,1.,0.));
#25459=DIRECTION('ref_axis',(0.942641491092022,0.,0.333806859234212));
#25460=DIRECTION('center_axis',(0.,-1.,0.));
#25461=DIRECTION('ref_axis',(0.942641491092022,0.,0.333806859234212));
#25462=DIRECTION('center_axis',(0.,1.,0.));
#25463=DIRECTION('ref_axis',(1.,0.,0.));
#25464=DIRECTION('',(-0.942641491091975,0.,0.333806859234346));
#25465=DIRECTION('center_axis',(0.,-1.,0.));
#25466=DIRECTION('ref_axis',(-0.942641491092032,0.,-0.333806859234184));
#25467=DIRECTION('',(0.942641491091975,0.,0.333806859234345));
#25468=DIRECTION('center_axis',(0.,1.,0.));
#25469=DIRECTION('ref_axis',(0.942641491092022,0.,0.333806859234212));
#25470=DIRECTION('center_axis',(0.,1.,0.));
#25471=DIRECTION('ref_axis',(0.942641491092022,0.,0.333806859234212));
#25472=DIRECTION('center_axis',(0.,1.,0.));
#25473=DIRECTION('ref_axis',(0.942641491092022,0.,0.333806859234212));
#25474=DIRECTION('',(-0.999440149526004,0.,-0.0334572490715973));
#25475=DIRECTION('center_axis',(0.,1.,0.));
#25476=DIRECTION('ref_axis',(0.942641491092022,0.,0.333806859234212));
#25477=DIRECTION('center_axis',(0.,1.,0.));
#25478=DIRECTION('ref_axis',(0.942641491092178,0.,0.333806859233771));
#25479=DIRECTION('center_axis',(0.,-1.,0.));
#25480=DIRECTION('ref_axis',(0.942641491092022,0.,0.333806859234212));
#25481=DIRECTION('',(0.,-1.,0.));
#25482=DIRECTION('center_axis',(0.,1.,0.));
#25483=DIRECTION('ref_axis',(0.942641491092178,0.,0.333806859233771));
#25484=DIRECTION('',(0.,1.,0.));
#25485=DIRECTION('center_axis',(0.,-1.,0.));
#25486=DIRECTION('ref_axis',(0.942641491092022,0.,0.333806859234212));
#25487=DIRECTION('center_axis',(0.0334572490706318,0.,-0.999440149526036));
#25488=DIRECTION('ref_axis',(0.,-1.,0.));
#25489=DIRECTION('',(0.999440149526004,0.,0.0334572490715973));
#25490=DIRECTION('center_axis',(0.,1.,0.));
#25491=DIRECTION('ref_axis',(0.942641491092178,0.,0.333806859233771));
#25492=DIRECTION('center_axis',(0.,-1.,0.));
#25493=DIRECTION('ref_axis',(0.942641491092022,0.,0.333806859234212));
#25494=DIRECTION('center_axis',(0.333806859233772,0.,0.942641491092178));
#25495=DIRECTION('ref_axis',(0.,-1.,0.));
#25496=DIRECTION('',(0.942641491091975,0.,-0.333806859234346));
#25497=DIRECTION('',(0.,1.,0.));
#25498=DIRECTION('center_axis',(0.,1.,0.));
#25499=DIRECTION('ref_axis',(-0.942641491092178,0.,-0.333806859233771));
#25500=DIRECTION('center_axis',(0.,1.,0.));
#25501=DIRECTION('ref_axis',(-0.942641491092032,0.,-0.333806859234184));
#25502=DIRECTION('',(0.,1.,0.));
#25503=DIRECTION('center_axis',(0.333806859233771,0.,-0.942641491092178));
#25504=DIRECTION('ref_axis',(0.,-1.,0.));
#25505=DIRECTION('',(-0.942641491091975,0.,-0.333806859234345));
#25506=DIRECTION('center_axis',(0.,1.,0.));
#25507=DIRECTION('ref_axis',(0.942641491092178,0.,0.333806859233771));
#25508=DIRECTION('center_axis',(0.,-1.,0.));
#25509=DIRECTION('ref_axis',(0.942641491092022,0.,0.333806859234212));
#25510=DIRECTION('center_axis',(0.,1.,0.));
#25511=DIRECTION('ref_axis',(1.,0.,0.));
#25512=DIRECTION('axis',(0.,0.,1.));
#25513=DIRECTION('refdir',(1.,0.,0.));
#25514=DIRECTION('center_axis',(6.65798752924967E-17,-1.,1.71022579061586E-31));
#25515=DIRECTION('ref_axis',(-0.211873077029416,-1.41064830464559E-17,0.97729719084324));
#25516=DIRECTION('',(-0.14981688951836,0.707106781186546,0.691053470879819));
#25517=DIRECTION('center_axis',(-6.65798752924967E-17,1.,-1.71022579061586E-31));
#25518=DIRECTION('ref_axis',(-0.211873077029416,-1.41064830464559E-17,0.977297190843239));
#25519=DIRECTION('center_axis',(-6.65798752924967E-17,1.,-1.71022579061586E-31));
#25520=DIRECTION('ref_axis',(-0.211873077029416,-1.41064830464559E-17,0.977297190843239));
#25521=DIRECTION('center_axis',(6.65798752924967E-17,-1.,1.71022579061586E-31));
#25522=DIRECTION('ref_axis',(-0.211873077029416,-1.41064830464559E-17,0.97729719084324));
#25523=DIRECTION('center_axis',(6.65798752924967E-17,-1.,1.71022579061586E-31));
#25524=DIRECTION('ref_axis',(-0.211873077029416,-1.41064830464559E-17,0.97729719084324));
#25525=DIRECTION('center_axis',(6.65798752924967E-17,-1.,1.71022579061586E-31));
#25526=DIRECTION('ref_axis',(-0.211873077029416,-1.41064830464559E-17,0.97729719084324));
#25527=DIRECTION('center_axis',(-6.65798752924967E-17,1.,-1.71022579061586E-31));
#25528=DIRECTION('ref_axis',(-0.211873077029416,-1.41064830464559E-17,0.977297190843239));
#25529=DIRECTION('center_axis',(-6.65798752924967E-17,1.,-1.71022579061586E-31));
#25530=DIRECTION('ref_axis',(0.211873077029416,1.41064830464559E-17,-0.977297190843239));
#25531=DIRECTION('center_axis',(6.65798752924967E-17,-1.,1.71022579061586E-31));
#25532=DIRECTION('ref_axis',(0.211873077029416,1.41064830464559E-17,-0.97729719084324));
#25533=DIRECTION('',(6.65798752924967E-17,-1.,1.71022579061586E-31));
#25534=DIRECTION('center_axis',(-6.65798752924967E-17,1.,-1.71022579061586E-31));
#25535=DIRECTION('ref_axis',(0.211873077029416,1.41064830464559E-17,-0.97729719084324));
#25536=DIRECTION('center_axis',(6.65798752924967E-17,-1.,1.71022579061586E-31));
#25537=DIRECTION('ref_axis',(0.97729719084324,6.50683250900503E-17,0.211873077029416));
#25538=DIRECTION('center_axis',(6.65798752924967E-17,-1.,1.71022579061586E-31));
#25539=DIRECTION('ref_axis',(0.211873077029416,1.41064830464559E-17,-0.977297190843239));
#25540=DIRECTION('center_axis',(6.65798752924967E-17,-1.,1.71022579061586E-31));
#25541=DIRECTION('ref_axis',(0.97729719084324,6.50683250900503E-17,0.211873077029416));
#25542=DIRECTION('center_axis',(-6.65798752924967E-17,1.,-1.71022579061586E-31));
#25543=DIRECTION('ref_axis',(0.211873077029416,1.41064830464559E-17,-0.977297190843239));
#25544=DIRECTION('center_axis',(-6.65798752924967E-17,1.,-1.71022579061586E-31));
#25545=DIRECTION('ref_axis',(0.211873077029416,1.41064830464559E-17,-0.97729719084324));
#25546=DIRECTION('',(-6.65798752924967E-17,1.,-1.71022579061586E-31));
#25547=DIRECTION('',(6.65798752924967E-17,-1.,1.71022579061586E-31));
#25548=DIRECTION('',(6.65798752924967E-17,-1.,1.71022579061586E-31));
#25549=DIRECTION('center_axis',(6.65798752924967E-17,-1.,1.71022579061586E-31));
#25550=DIRECTION('ref_axis',(0.211873077029416,1.41064830464559E-17,-0.977297190843239));
#25551=DIRECTION('center_axis',(-0.97729719084324,-6.50683250900503E-17,
-0.211873077029416));
#25552=DIRECTION('ref_axis',(-0.211873077029416,-1.06625068431886E-16,0.97729719084324));
#25553=DIRECTION('',(0.211873077028438,1.41064830463908E-17,-0.977297190843451));
#25554=DIRECTION('center_axis',(6.65798752924967E-17,-1.,1.71022579061586E-31));
#25555=DIRECTION('ref_axis',(0.97729719084324,6.50683250900503E-17,0.211873077029416));
#25556=DIRECTION('center_axis',(-6.65798752924967E-17,1.,-1.71022579061586E-31));
#25557=DIRECTION('ref_axis',(0.211873077029416,1.41064830464559E-17,-0.97729719084324));
#25558=DIRECTION('',(6.65798752924967E-17,-1.,1.71022579061586E-31));
#25559=DIRECTION('center_axis',(6.65798752924967E-17,-1.,1.71022579061586E-31));
#25560=DIRECTION('ref_axis',(-0.211873077029416,-1.41064830464559E-17,0.977297190843239));
#25561=DIRECTION('center_axis',(6.65798752924967E-17,-1.,1.71022579061586E-31));
#25562=DIRECTION('ref_axis',(-0.211873077029416,-1.41064830464559E-17,0.977297190843239));
#25563=DIRECTION('center_axis',(-6.65798752924967E-17,1.,-1.71022579061586E-31));
#25564=DIRECTION('ref_axis',(-0.211873077029416,-1.41064830464559E-17,0.97729719084324));
#25565=DIRECTION('',(-0.14981688951836,-0.707106781186546,0.691053470879819));
#25566=DIRECTION('center_axis',(-6.65798752924967E-17,1.,-1.71022579061586E-31));
#25567=DIRECTION('ref_axis',(-0.211873077029416,-1.41064830464559E-17,0.97729719084324));
#25568=DIRECTION('center_axis',(-6.65798752924967E-17,1.,-1.71022579061586E-31));
#25569=DIRECTION('ref_axis',(-0.211873077029416,-1.41064830464559E-17,0.97729719084324));
#25570=DIRECTION('center_axis',(-6.65798752924967E-17,1.,-1.71022579061586E-31));
#25571=DIRECTION('ref_axis',(-0.211873077029416,-1.41064830464559E-17,0.97729719084324));
#25572=DIRECTION('axis',(0.,0.,1.));
#25573=DIRECTION('refdir',(1.,0.,0.));
#25574=DIRECTION('center_axis',(-1.,0.,-8.67628499512335E-13));
#25575=DIRECTION('ref_axis',(8.67628499512335E-13,-5.79319727271681E-31,
-1.));
#25576=DIRECTION('',(8.67628499512335E-13,5.22733802929053E-29,-1.));
#25577=DIRECTION('',(0.,-1.,0.));
#25578=DIRECTION('',(-8.67628499512335E-13,-5.22733802929053E-29,1.));
#25579=DIRECTION('',(6.4098735490554E-44,-1.,-7.38780889823027E-32));
#25580=DIRECTION('center_axis',(-1.,0.,-8.67628499512335E-13));
#25581=DIRECTION('ref_axis',(8.67628499512335E-13,-5.79319727271681E-31,
-1.));
#25582=DIRECTION('',(-8.67628499512335E-13,-5.22733802929053E-29,1.));
#25583=DIRECTION('',(0.,1.,0.));
#25584=DIRECTION('',(8.67628499512335E-13,5.22733802929053E-29,-1.));
#25585=DIRECTION('',(-5.24091500843978E-44,1.,6.04050582868765E-32));
#25586=DIRECTION('center_axis',(4.64905891561784E-16,0.,1.));
#25587=DIRECTION('ref_axis',(-1.,-2.80259692864963E-45,4.64905891561784E-16));
#25588=DIRECTION('',(-1.,-6.02124417212377E-17,4.64905891561784E-16));
#25589=DIRECTION('',(-6.02124417212377E-17,1.,2.7993118901524E-32));
#25590=DIRECTION('',(1.,6.02124417212377E-17,-4.64905891561784E-16));
#25591=DIRECTION('center_axis',(-4.64905891561784E-16,0.,-1.));
#25592=DIRECTION('ref_axis',(1.,2.80259692864963E-45,-4.64905891561784E-16));
#25593=DIRECTION('',(-1.,-6.02124417212377E-17,4.64905891561784E-16));
#25594=DIRECTION('',(6.02124417212377E-17,-1.,-2.7993118901524E-32));
#25595=DIRECTION('',(1.,6.02124417212377E-17,-4.64905891561784E-16));
#25596=DIRECTION('center_axis',(7.06303505265682E-16,7.38780889823027E-32,
-1.));
#25597=DIRECTION('ref_axis',(-1.,-6.02124417212377E-17,-7.06303505265682E-16));
#25598=DIRECTION('',(-1.,-6.02124417212377E-17,-7.06303505265682E-16));
#25599=DIRECTION('',(-6.02124417212377E-17,1.,3.1349830333987E-32));
#25600=DIRECTION('',(-1.,-6.02124417212377E-17,-7.06303505265682E-16));
#25601=DIRECTION('center_axis',(-6.02124417212377E-17,1.,3.1349830333987E-32));
#25602=DIRECTION('ref_axis',(-7.06303505265682E-16,-7.38780889823028E-32,
1.));
#25603=DIRECTION('',(9.99517454745522E-13,6.01520366628906E-29,1.));
#25604=DIRECTION('',(-1.,-6.02124417212377E-17,9.99517454745522E-13));
#25605=DIRECTION('',(-0.691222645967388,-4.16202032867111E-17,0.722641857147676));
#25606=DIRECTION('',(-1.,-6.02124417212377E-17,9.99834661323986E-13));
#25607=DIRECTION('',(1.00090892313815E-12,6.02985200330567E-29,-1.));
#25608=DIRECTION('center_axis',(6.02124417212377E-17,-1.,-3.1349830333987E-32));
#25609=DIRECTION('ref_axis',(-7.06303505265682E-16,-7.38780889823028E-32,
1.));
#25610=DIRECTION('',(9.99720074379408E-13,6.01642368857876E-29,1.));
#25611=DIRECTION('',(-1.,-6.02124417212377E-17,-1.00102351008273E-12));
#25612=DIRECTION('',(-0.691222645967387,-4.1620203286711E-17,-0.722641857147678));
#25613=DIRECTION('center_axis',(4.82545253477761E-16,6.04050582868765E-32,
-1.));
#25614=DIRECTION('ref_axis',(-6.02124417212377E-17,1.,3.13498303339869E-32));
#25615=DIRECTION('',(-1.,-6.02124417212377E-17,9.99517454745522E-13));
#25616=DIRECTION('',(-6.02124417212377E-17,1.,3.1349830333987E-32));
#25617=DIRECTION('center_axis',(1.,6.02124417212377E-17,9.08923139152315E-16));
#25618=DIRECTION('ref_axis',(6.02124417212377E-17,-1.,-3.1349830333987E-32));
#25619=DIRECTION('',(-6.02124417212377E-17,1.,3.1349830333987E-32));
#25620=DIRECTION('',(1.00090892313815E-12,6.02985200330567E-29,-1.));
#25621=DIRECTION('',(-6.02124417212377E-17,1.,3.1349830333987E-32));
#25622=DIRECTION('center_axis',(1.6533867501343E-16,4.13052756674997E-32,
-1.));
#25623=DIRECTION('ref_axis',(-6.02124417212377E-17,1.,3.13498303339869E-32));
#25624=DIRECTION('',(-6.02124417212377E-17,1.,3.1349830333987E-32));
#25625=DIRECTION('',(-1.,-6.02124417212377E-17,9.99834661323986E-13));
#25626=DIRECTION('center_axis',(-0.722641857147698,-4.35120307088327E-17,
-0.691222645967365));
#25627=DIRECTION('ref_axis',(-6.02124417212376E-17,1.,9.19638474680743E-32));
#25628=DIRECTION('',(-0.691222645967388,-4.16202032867111E-17,0.722641857147676));
#25629=DIRECTION('center_axis',(1.,6.02124417212377E-17,7.06303505265682E-16));
#25630=DIRECTION('ref_axis',(6.02124417212377E-17,-1.,-3.1349830333987E-32));
#25631=DIRECTION('',(9.99517454745522E-13,6.01520366628906E-29,1.));
#25632=DIRECTION('center_axis',(-6.02124417212377E-17,1.,3.1349830333987E-32));
#25633=DIRECTION('ref_axis',(1.,6.02124417212377E-17,7.6753584522305E-16));
#25634=DIRECTION('center_axis',(6.02124417212377E-17,-1.,-3.1349830333987E-32));
#25635=DIRECTION('ref_axis',(-7.06303505265682E-16,-7.38780889823028E-32,
1.));
#25636=DIRECTION('',(-6.02124417212377E-17,1.,3.1349830333987E-32));
#25637=DIRECTION('center_axis',(-1.,-6.02124417212375E-17,-7.06303505265682E-16));
#25638=DIRECTION('ref_axis',(-7.06303505265682E-16,-4.26377885674554E-16,
1.));
#25639=DIRECTION('',(9.99720074379408E-13,6.01642368857876E-29,1.));
#25640=DIRECTION('',(-6.02124417212377E-17,1.,3.1349830333987E-32));
#25641=DIRECTION('center_axis',(1.02351008373001E-15,9.29778716016794E-32,
-1.));
#25642=DIRECTION('ref_axis',(-1.,-6.02124417212377E-17,-1.02351008373001E-15));
#25643=DIRECTION('',(-1.,-6.02124417212377E-17,-1.00102351008273E-12));
#25644=DIRECTION('',(-6.02124417212377E-17,1.,3.1349830333987E-32));
#25645=DIRECTION('center_axis',(0.7226418571477,4.35120307088328E-17,-0.691222645967364));
#25646=DIRECTION('ref_axis',(-0.691222645967364,-4.16202032867096E-17,-0.7226418571477));
#25647=DIRECTION('',(-0.691222645967387,-4.1620203286711E-17,-0.722641857147678));
#25648=DIRECTION('center_axis',(-6.02124417212377E-17,1.,3.1349830333987E-32));
#25649=DIRECTION('ref_axis',(-7.06303505265682E-16,-7.38780889823028E-32,
1.));
#25650=DIRECTION('axis',(0.,0.,1.));
#25651=DIRECTION('refdir',(1.,0.,0.));
#25652=DIRECTION('center_axis',(4.57029560239561E-17,1.,8.81733986229836E-18));
#25653=DIRECTION('ref_axis',(4.44089209850056E-15,-8.81733986229857E-18,
1.));
#25654=DIRECTION('center_axis',(4.57029560239561E-17,1.,8.81733986229836E-18));
#25655=DIRECTION('ref_axis',(4.44089209850056E-15,-8.81733986229857E-18,
1.));
#25656=DIRECTION('',(4.57029560239561E-17,1.,8.81733986229836E-18));
#25657=DIRECTION('center_axis',(-4.57029560239561E-17,-1.,-8.81733986229836E-18));
#25658=DIRECTION('ref_axis',(4.44089209850056E-15,-8.81733986229857E-18,
1.));
#25659=DIRECTION('center_axis',(4.57029560239561E-17,1.,8.81733986229836E-18));
#25660=DIRECTION('ref_axis',(4.44089209850056E-15,-8.81733986229857E-18,
1.));
#25661=DIRECTION('center_axis',(4.57029560239561E-17,1.,8.81733986229836E-18));
#25662=DIRECTION('ref_axis',(4.44089209850056E-15,-8.81733986229857E-18,
1.));
#25663=DIRECTION('',(4.57029560239561E-17,1.,8.81733986229836E-18));
#25664=DIRECTION('center_axis',(-4.57029560239561E-17,-1.,-8.81733986229836E-18));
#25665=DIRECTION('ref_axis',(4.44089209850056E-15,-8.81733986229857E-18,
1.));
#25666=DIRECTION('center_axis',(4.57029560239561E-17,1.,8.81733986229836E-18));
#25667=DIRECTION('ref_axis',(4.44089209850056E-15,-8.81733986229857E-18,
1.));
#25668=DIRECTION('center_axis',(4.57029560239561E-17,1.,8.81733986229836E-18));
#25669=DIRECTION('ref_axis',(4.44089209850056E-15,-8.81733986229857E-18,
1.));
#25670=DIRECTION('',(4.57029560239561E-17,1.,8.81733986229836E-18));
#25671=DIRECTION('center_axis',(-4.57029560239561E-17,-1.,-8.81733986229836E-18));
#25672=DIRECTION('ref_axis',(4.44089209850056E-15,-8.81733986229857E-18,
1.));
#25673=DIRECTION('center_axis',(4.57029560239561E-17,1.,8.81733986229836E-18));
#25674=DIRECTION('ref_axis',(4.44089209850056E-15,-8.81733986229857E-18,
1.));
#25675=DIRECTION('center_axis',(4.57029560239561E-17,1.,8.81733986229836E-18));
#25676=DIRECTION('ref_axis',(4.44089209850056E-15,-8.81733986229857E-18,
1.));
#25677=DIRECTION('',(4.57029560239561E-17,1.,8.81733986229836E-18));
#25678=DIRECTION('center_axis',(-4.57029560239561E-17,-1.,-8.81733986229836E-18));
#25679=DIRECTION('ref_axis',(4.44089209850056E-15,-8.81733986229857E-18,
1.));
#25680=DIRECTION('center_axis',(4.57029560239561E-17,1.,8.81733986229836E-18));
#25681=DIRECTION('ref_axis',(4.44089209850056E-15,-8.81733986229857E-18,
1.));
#25682=DIRECTION('center_axis',(4.57029560239561E-17,1.,8.81733986229836E-18));
#25683=DIRECTION('ref_axis',(4.44089209850056E-15,-8.81733986229856E-18,
1.));
#25684=DIRECTION('',(4.57029560239561E-17,1.,8.81733986229836E-18));
#25685=DIRECTION('center_axis',(-4.57029560239561E-17,-1.,-8.81733986229836E-18));
#25686=DIRECTION('ref_axis',(4.44089209850056E-15,-8.81733986229856E-18,
1.));
#25687=DIRECTION('center_axis',(4.57029560239561E-17,1.,8.81733986229836E-18));
#25688=DIRECTION('ref_axis',(4.44089209850056E-15,-8.81733986229857E-18,
1.));
#25689=DIRECTION('center_axis',(4.57029560239561E-17,1.,8.81733986229836E-18));
#25690=DIRECTION('ref_axis',(4.44089209850056E-15,-8.81733986229856E-18,
1.));
#25691=DIRECTION('',(4.57029560239561E-17,1.,8.81733986229836E-18));
#25692=DIRECTION('center_axis',(-4.57029560239561E-17,-1.,-8.81733986229836E-18));
#25693=DIRECTION('ref_axis',(4.44089209850056E-15,-8.81733986229856E-18,
1.));
#25694=DIRECTION('center_axis',(4.57029560239561E-17,1.,8.81733986229836E-18));
#25695=DIRECTION('ref_axis',(4.44089209850056E-15,-8.81733986229857E-18,
1.));
#25696=DIRECTION('center_axis',(4.57029560239561E-17,1.,8.81733986229836E-18));
#25697=DIRECTION('ref_axis',(4.44089209850056E-15,-8.81733986229856E-18,
1.));
#25698=DIRECTION('',(4.57029560239561E-17,1.,8.81733986229836E-18));
#25699=DIRECTION('center_axis',(-4.57029560239561E-17,-1.,-8.81733986229836E-18));
#25700=DIRECTION('ref_axis',(4.44089209850056E-15,-8.81733986229856E-18,
1.));
#25701=DIRECTION('center_axis',(4.57029560239561E-17,1.,8.81733986229836E-18));
#25702=DIRECTION('ref_axis',(4.44089209850056E-15,-8.81733986229857E-18,
1.));
#25703=DIRECTION('center_axis',(4.57029560239561E-17,1.,8.81733986229836E-18));
#25704=DIRECTION('ref_axis',(4.44089209850056E-15,-8.81733986229856E-18,
1.));
#25705=DIRECTION('',(4.57029560239561E-17,1.,8.81733986229836E-18));
#25706=DIRECTION('center_axis',(-4.57029560239561E-17,-1.,-8.81733986229836E-18));
#25707=DIRECTION('ref_axis',(4.44089209850056E-15,-8.81733986229856E-18,
1.));
#25708=DIRECTION('center_axis',(4.57029560239561E-17,1.,8.81733986229836E-18));
#25709=DIRECTION('ref_axis',(4.44089209850056E-15,-8.81733986229857E-18,
1.));
#25710=DIRECTION('center_axis',(4.57029560239561E-17,1.,8.81733986229836E-18));
#25711=DIRECTION('ref_axis',(4.44089209850056E-15,-8.81733986229856E-18,
1.));
#25712=DIRECTION('',(4.57029560239561E-17,1.,8.81733986229836E-18));
#25713=DIRECTION('center_axis',(-4.57029560239561E-17,-1.,-8.81733986229836E-18));
#25714=DIRECTION('ref_axis',(4.44089209850056E-15,-8.81733986229856E-18,
1.));
#25715=DIRECTION('center_axis',(4.57029560239561E-17,1.,8.81733986229836E-18));
#25716=DIRECTION('ref_axis',(4.44089209850056E-15,-8.81733986229857E-18,
1.));
#25717=DIRECTION('center_axis',(4.57029560239561E-17,1.,8.81733986229836E-18));
#25718=DIRECTION('ref_axis',(4.44089209850056E-15,-8.81733986229856E-18,
1.));
#25719=DIRECTION('',(4.57029560239561E-17,1.,8.81733986229836E-18));
#25720=DIRECTION('center_axis',(-4.57029560239561E-17,-1.,-8.81733986229836E-18));
#25721=DIRECTION('ref_axis',(4.44089209850056E-15,-8.81733986229856E-18,
1.));
#25722=DIRECTION('center_axis',(-0.704142011834323,3.84422044398024E-17,
-0.71005917159763));
#25723=DIRECTION('ref_axis',(4.57029560239561E-17,1.,8.81733986229838E-18));
#25724=DIRECTION('',(-0.710059171597626,2.62431436642672E-17,0.704142011834327));
#25725=DIRECTION('',(4.57029560239561E-17,1.,8.81733986229836E-18));
#25726=DIRECTION('',(-0.710059171597626,2.62431436642672E-17,0.704142011834327));
#25727=DIRECTION('',(4.57029560239561E-17,1.,8.81733986229836E-18));
#25728=DIRECTION('center_axis',(-4.69798701365815E-15,8.81733986229857E-18,
-1.));
#25729=DIRECTION('ref_axis',(4.57029560239561E-17,1.,8.81733986229836E-18));
#25730=DIRECTION('',(-1.,4.57029560239473E-17,1.00469798701266E-12));
#25731=DIRECTION('',(4.57029560239561E-17,1.,8.81733986229836E-18));
#25732=DIRECTION('',(-1.,4.57029560239473E-17,1.00469798701266E-12));
#25733=DIRECTION('center_axis',(1.,-4.57029560239561E-17,-4.42423575072469E-15));
#25734=DIRECTION('ref_axis',(-4.57029560239561E-17,-1.,-8.81733986229836E-18));
#25735=DIRECTION('',(9.95575764248275E-13,8.81733986225286E-18,-1.));
#25736=DIRECTION('',(4.57029560239561E-17,1.,8.81733986229836E-18));
#25737=DIRECTION('',(9.95575764248275E-13,8.81733986225286E-18,-1.));
#25738=DIRECTION('',(4.57029560239561E-17,1.,8.81733986229836E-18));
#25739=DIRECTION('center_axis',(-4.49871621436646E-15,8.81733986229856E-18,
-1.));
#25740=DIRECTION('ref_axis',(4.57029560239561E-17,1.,8.81733986229835E-18));
#25741=DIRECTION('',(-1.,4.57029560239473E-17,1.00449871621337E-12));
#25742=DIRECTION('',(-1.,4.57029560239473E-17,1.00449871621337E-12));
#25743=DIRECTION('center_axis',(0.704142011834316,-2.59205383631653E-17,
-0.710059171597636));
#25744=DIRECTION('ref_axis',(-0.710059171597636,3.86604625235991E-17,-0.704142011834316));
#25745=DIRECTION('',(-0.710059171597632,3.8660462523599E-17,-0.704142011834321));
#25746=DIRECTION('',(4.57029560239561E-17,1.,8.81733986229836E-18));
#25747=DIRECTION('',(-0.710059171597632,3.8660462523599E-17,-0.704142011834321));
#25748=DIRECTION('',(4.57029560239561E-17,1.,8.81733986229836E-18));
#25749=DIRECTION('center_axis',(-4.61169564075059E-15,8.81733986229857E-18,
-1.));
#25750=DIRECTION('ref_axis',(4.57029560239561E-17,1.,8.81733986229836E-18));
#25751=DIRECTION('',(-1.,4.57029560239473E-17,1.00461169563975E-12));
#25752=DIRECTION('',(-1.,4.57029560239473E-17,1.00461169563975E-12));
#25753=DIRECTION('',(4.57029560239561E-17,1.,8.81733986229836E-18));
#25754=DIRECTION('center_axis',(1.,-4.57029560239561E-17,-4.44089209850056E-15));
#25755=DIRECTION('ref_axis',(-4.57029560239561E-17,-1.,-8.81733986229836E-18));
#25756=DIRECTION('',(1.00486879055491E-12,-8.81733986234428E-18,1.));
#25757=DIRECTION('',(1.00486879055491E-12,-8.81733986234428E-18,1.));
#25758=DIRECTION('center_axis',(4.57029560239561E-17,1.,8.81733986229836E-18));
#25759=DIRECTION('ref_axis',(4.44089209850056E-15,-8.81733986229856E-18,
1.));
#25760=DIRECTION('center_axis',(-4.57029560239561E-17,-1.,-8.81733986229836E-18));
#25761=DIRECTION('ref_axis',(4.44089209850056E-15,-8.81733986229856E-18,
1.));
#25762=DIRECTION('center_axis',(-4.57029560239561E-17,-1.,-8.81733986229836E-18));
#25763=DIRECTION('ref_axis',(4.44089209850056E-15,-8.81733986229856E-18,
1.));
#25764=DIRECTION('',(4.57029560239561E-17,1.,8.81733986229836E-18));
#25765=DIRECTION('center_axis',(-1.,4.57029560239563E-17,4.44089209850056E-15));
#25766=DIRECTION('ref_axis',(4.44089209850056E-15,-4.5337214504578E-16,
1.));
#25767=DIRECTION('',(1.00488544690268E-12,-8.81733986234428E-18,1.));
#25768=DIRECTION('',(1.00488544690268E-12,-8.81733986234428E-18,1.));
#25769=DIRECTION('',(4.57029560239561E-17,1.,8.81733986229836E-18));
#25770=DIRECTION('center_axis',(-4.81096644004228E-15,8.81733986229858E-18,
-1.));
#25771=DIRECTION('ref_axis',(4.57029560239561E-17,1.,8.81733986229836E-18));
#25772=DIRECTION('',(-1.,4.57029560239473E-17,1.00481096643904E-12));
#25773=DIRECTION('',(-1.,4.57029560239473E-17,1.00481096643904E-12));
#25774=DIRECTION('center_axis',(4.57029560239561E-17,1.,8.81733986229836E-18));
#25775=DIRECTION('ref_axis',(4.44089209850056E-15,-8.81733986229856E-18,
1.));
#25776=DIRECTION('center_axis',(4.57029560239561E-17,1.,8.81733986229836E-18));
#25777=DIRECTION('ref_axis',(4.44089209850056E-15,-8.81733986229856E-18,
1.));
#25778=DIRECTION('axis',(0.,0.,1.));
#25779=DIRECTION('refdir',(1.,0.,0.));
#25780=DIRECTION('center_axis',(1.,5.1420277733694E-16,-1.0522467400333E-14));
#25781=DIRECTION('ref_axis',(-1.0522467400333E-14,1.06077175752244E-14,
-1.));
#25782=DIRECTION('',(-1.00001914094642E-12,1.00113222673461E-12,1.));
#25783=DIRECTION('',(-9.47915311079142E-15,-1.,1.E-14));
#25784=DIRECTION('',(1.00001914094642E-12,-9.99999999998997E-13,-1.));
#25785=DIRECTION('',(-9.47915311079142E-15,-1.,1.E-14));
#25786=DIRECTION('center_axis',(-4.5961454925099E-16,1.,6.61092274672771E-17));
#25787=DIRECTION('ref_axis',(-1.05885766278003E-14,6.61092274672722E-17,
-1.));
#25788=DIRECTION('',(1.,-9.54038545074888E-15,9.9999999999998E-15));
#25789=DIRECTION('',(-9.56631913100564E-15,9.99999999999985E-15,1.));
#25790=DIRECTION('',(-1.,9.54038545074888E-15,-9.9999999999998E-15));
#25791=DIRECTION('center_axis',(0.,-4.29362650667545E-31,1.));
#25792=DIRECTION('ref_axis',(4.28756753891971E-16,-1.,-4.29362650667545E-31));
#25793=DIRECTION('',(-9.99999999999976E-15,-1.04336808689941E-14,1.));
#25794=DIRECTION('center_axis',(-1.99999999991998E-11,2.E-11,1.));
#25795=DIRECTION('ref_axis',(-1.99995712428458E-11,-1.,1.99999999996E-11));
#25796=DIRECTION('',(-9.56631913100564E-15,9.99999999999985E-15,1.));
#25797=DIRECTION('center_axis',(-1.99999999991998E-11,2.E-11,1.));
#25798=DIRECTION('ref_axis',(-1.99995712428458E-11,-1.,1.99999999996E-11));
#25799=DIRECTION('center_axis',(1.,5.2084688920845E-16,-1.0522467400333E-14));
#25800=DIRECTION('ref_axis',(-1.0522467400333E-14,1.01548957588061E-14,
-1.));
#25801=DIRECTION('',(-9.47915311079142E-15,-1.,1.E-14));
#25802=DIRECTION('',(-9.47915311079142E-15,-1.,1.E-14));
#25803=DIRECTION('center_axis',(-5.3389151001177E-16,1.,6.61092274672778E-17));
#25804=DIRECTION('ref_axis',(-1.06105803387953E-14,6.61092274672721E-17,
-1.));
#25805=DIRECTION('',(-1.,9.99485333130104E-13,-1.00005108521413E-12));
#25806=DIRECTION('',(-9.99999999998993E-13,1.00002200370999E-12,1.));
#25807=DIRECTION('',(1.,-9.99466108488984E-13,9.99906900405741E-13));
#25808=DIRECTION('center_axis',(-1.0522467400333E-14,2.19844233825538E-15,
-1.));
#25809=DIRECTION('ref_axis',(1.,-6.53116410123922E-15,-1.0522467400333E-14));
#25810=DIRECTION('',(9.99479153109799E-13,1.,1.00219844233724E-12));
#25811=DIRECTION('',(1.,-9.99466108488984E-13,9.99906900405741E-13));
#25812=DIRECTION('center_axis',(5.33891510011771E-16,-1.,2.20037109950003E-17));
#25813=DIRECTION('ref_axis',(-1.,-5.33891510011771E-16,1.0522467400333E-14));
#25814=DIRECTION('',(9.99999999998993E-13,-1.00002200370999E-12,-1.));
#25815=DIRECTION('',(1.,-9.99466108488984E-13,9.99906900405741E-13));
#25816=DIRECTION('center_axis',(9.30995932482184E-17,-4.41888838750562E-15,
1.));
#25817=DIRECTION('ref_axis',(1.,3.89820370584558E-15,-9.30995932482012E-17));
#25818=DIRECTION('',(-9.99479153109799E-13,-1.,-1.00441888838649E-12));
#25819=DIRECTION('center_axis',(1.,5.3389151001188E-16,-1.0522467400333E-14));
#25820=DIRECTION('ref_axis',(-1.0522467400333E-14,1.04954770345521E-14,
-1.));
#25821=DIRECTION('axis',(0.,0.,1.));
#25822=DIRECTION('refdir',(1.,0.,0.));
#25823=DIRECTION('center_axis',(0.,-1.,0.));
#25824=DIRECTION('ref_axis',(0.281918008728675,0.,-0.959438500558769));
#25825=DIRECTION('center_axis',(0.,1.,0.));
#25826=DIRECTION('ref_axis',(0.281918008754676,0.,-0.959438500551129));
#25827=DIRECTION('',(0.,-1.,0.));
#25828=DIRECTION('center_axis',(0.,-1.,0.));
#25829=DIRECTION('ref_axis',(0.281918008754676,0.,-0.959438500551129));
#25830=DIRECTION('',(0.,1.,0.));
#25831=DIRECTION('center_axis',(0.,-1.,0.));
#25832=DIRECTION('ref_axis',(-0.470745247127108,0.,-0.882269183586981));
#25833=DIRECTION('center_axis',(0.,-1.,0.));
#25834=DIRECTION('ref_axis',(-0.470745247127378,0.,-0.882269183586837));
#25835=DIRECTION('',(0.,1.,0.));
#25836=DIRECTION('center_axis',(0.,1.,0.));
#25837=DIRECTION('ref_axis',(-0.470745247127378,0.,-0.882269183586837));
#25838=DIRECTION('center_axis',(0.,-1.,0.));
#25839=DIRECTION('ref_axis',(-0.971857119217081,0.,-0.235571092936032));
#25840=DIRECTION('center_axis',(0.,1.,0.));
#25841=DIRECTION('ref_axis',(-0.971857119210143,0.,-0.235571092964655));
#25842=DIRECTION('',(0.,-1.,0.));
#25843=DIRECTION('center_axis',(0.,-1.,0.));
#25844=DIRECTION('ref_axis',(-0.971857119210143,0.,-0.235571092964655));
#25845=DIRECTION('center_axis',(-0.848811934516349,0.,0.528694902398929));
#25846=DIRECTION('ref_axis',(0.,1.,0.));
#25847=DIRECTION('',(-0.528694902399201,0.,-0.84881193451618));
#25848=DIRECTION('',(0.,1.,0.));
#25849=DIRECTION('',(0.528694902399201,0.,0.84881193451618));
#25850=DIRECTION('center_axis',(0.,-1.,0.));
#25851=DIRECTION('ref_axis',(0.154274306935528,0.,-0.988028055380799));
#25852=DIRECTION('center_axis',(0.,1.,0.));
#25853=DIRECTION('ref_axis',(0.154274306968479,0.,-0.988028055375654));
#25854=DIRECTION('',(0.,-1.,0.));
#25855=DIRECTION('center_axis',(0.,-1.,0.));
#25856=DIRECTION('ref_axis',(0.154274306968479,0.,-0.988028055375654));
#25857=DIRECTION('',(0.,1.,0.));
#25858=DIRECTION('center_axis',(0.,-1.,0.));
#25859=DIRECTION('ref_axis',(-0.581877193327018,0.,-0.813276663802591));
#25860=DIRECTION('center_axis',(0.,-1.,0.));
#25861=DIRECTION('ref_axis',(-0.581877193327158,0.,-0.813276663802491));
#25862=DIRECTION('',(0.,1.,0.));
#25863=DIRECTION('center_axis',(0.,1.,0.));
#25864=DIRECTION('ref_axis',(-0.581877193327158,0.,-0.813276663802491));
#25865=DIRECTION('center_axis',(0.,-1.,0.));
#25866=DIRECTION('ref_axis',(-0.994290944595386,0.,-0.106702940426286));
#25867=DIRECTION('center_axis',(0.,1.,0.));
#25868=DIRECTION('ref_axis',(-0.994290944591597,0.,-0.106702940461587));
#25869=DIRECTION('',(0.,-1.,0.));
#25870=DIRECTION('center_axis',(0.,-1.,0.));
#25871=DIRECTION('ref_axis',(-0.994290944591597,0.,-0.106702940461587));
#25872=DIRECTION('center_axis',(-0.772541698292714,0.,0.634964033941301));
#25873=DIRECTION('ref_axis',(0.,1.,0.));
#25874=DIRECTION('',(-0.634964033941407,0.,-0.772541698292626));
#25875=DIRECTION('',(0.,1.,0.));
#25876=DIRECTION('',(0.634964033941407,0.,0.772541698292626));
#25877=DIRECTION('center_axis',(0.,-1.,0.));
#25878=DIRECTION('ref_axis',(0.0239909289777922,0.,-0.999712176242133));
#25879=DIRECTION('center_axis',(0.,1.,0.));
#25880=DIRECTION('ref_axis',(0.0239909290168098,0.,-0.999712176241197));
#25881=DIRECTION('',(0.,-1.,0.));
#25882=DIRECTION('center_axis',(0.,-1.,0.));
#25883=DIRECTION('ref_axis',(0.0239909290168098,0.,-0.999712176241197));
#25884=DIRECTION('',(0.,1.,0.));
#25885=DIRECTION('center_axis',(0.,-1.,0.));
#25886=DIRECTION('ref_axis',(-0.683053059422266,0.,-0.730368754817648));
#25887=DIRECTION('center_axis',(0.,-1.,0.));
#25888=DIRECTION('ref_axis',(-0.683053059422292,0.,-0.730368754817624));
#25889=DIRECTION('',(0.,1.,0.));
#25890=DIRECTION('center_axis',(0.,1.,0.));
#25891=DIRECTION('ref_axis',(-0.683053059422292,0.,-0.730368754817624));
#25892=DIRECTION('center_axis',(0.,-1.,0.));
#25893=DIRECTION('ref_axis',(-0.999712176242133,0.,0.0239909289777984));
#25894=DIRECTION('center_axis',(0.,1.,0.));
#25895=DIRECTION('ref_axis',(-0.999712176241197,0.,0.023990929016816));
#25896=DIRECTION('',(0.,-1.,0.));
#25897=DIRECTION('center_axis',(0.,-1.,0.));
#25898=DIRECTION('ref_axis',(-0.999712176241197,0.,0.023990929016816));
#25899=DIRECTION('center_axis',(-0.683053059422266,0.,0.730368754817649));
#25900=DIRECTION('ref_axis',(0.,1.,0.));
#25901=DIRECTION('',(-0.730368754817616,0.,-0.6830530594223));
#25902=DIRECTION('',(0.,1.,0.));
#25903=DIRECTION('',(0.730368754817616,0.,0.6830530594223));
#25904=DIRECTION('center_axis',(0.,-1.,0.));
#25905=DIRECTION('ref_axis',(-0.106702940426286,0.,-0.994290944595386));
#25906=DIRECTION('center_axis',(0.,1.,0.));
#25907=DIRECTION('ref_axis',(-0.106702940461587,0.,-0.994290944591597));
#25908=DIRECTION('',(0.,-1.,0.));
#25909=DIRECTION('center_axis',(0.,-1.,0.));
#25910=DIRECTION('ref_axis',(-0.106702940461587,0.,-0.994290944591597));
#25911=DIRECTION('',(0.,1.,0.));
#25912=DIRECTION('center_axis',(0.,-1.,0.));
#25913=DIRECTION('ref_axis',(-0.772541698292714,0.,-0.634964033941301));
#25914=DIRECTION('center_axis',(0.,-1.,0.));
#25915=DIRECTION('ref_axis',(-0.772541698292649,0.,-0.63496403394138));
#25916=DIRECTION('',(0.,1.,0.));
#25917=DIRECTION('center_axis',(0.,1.,0.));
#25918=DIRECTION('ref_axis',(-0.772541698292649,0.,-0.63496403394138));
#25919=DIRECTION('center_axis',(0.,-1.,0.));
#25920=DIRECTION('ref_axis',(-0.988028055380799,0.,0.154274306935524));
#25921=DIRECTION('center_axis',(0.,1.,0.));
#25922=DIRECTION('ref_axis',(-0.988028055375654,0.,0.154274306968475));
#25923=DIRECTION('',(0.,-1.,0.));
#25924=DIRECTION('center_axis',(0.,-1.,0.));
#25925=DIRECTION('ref_axis',(-0.988028055375654,0.,0.154274306968475));
#25926=DIRECTION('center_axis',(-0.581877193327017,0.,0.813276663802591));
#25927=DIRECTION('ref_axis',(0.,1.,0.));
#25928=DIRECTION('',(-0.813276663802457,0.,-0.581877193327205));
#25929=DIRECTION('',(0.,1.,0.));
#25930=DIRECTION('',(0.813276663802457,0.,0.581877193327205));
#25931=DIRECTION('center_axis',(0.,-1.,0.));
#25932=DIRECTION('ref_axis',(-0.235571092936033,0.,-0.971857119217081));
#25933=DIRECTION('center_axis',(0.,1.,0.));
#25934=DIRECTION('ref_axis',(-0.235571092964656,0.,-0.971857119210143));
#25935=DIRECTION('',(0.,-1.,0.));
#25936=DIRECTION('center_axis',(0.,-1.,0.));
#25937=DIRECTION('ref_axis',(-0.235571092964656,0.,-0.971857119210143));
#25938=DIRECTION('',(0.,1.,0.));
#25939=DIRECTION('center_axis',(0.,-1.,0.));
#25940=DIRECTION('ref_axis',(-0.848811934516349,0.,-0.528694902398929));
#25941=DIRECTION('center_axis',(0.,-1.,0.));
#25942=DIRECTION('ref_axis',(-0.848811934516223,0.,-0.528694902399131));
#25943=DIRECTION('',(0.,1.,0.));
#25944=DIRECTION('center_axis',(0.,1.,0.));
#25945=DIRECTION('ref_axis',(-0.848811934516223,0.,-0.528694902399131));
#25946=DIRECTION('center_axis',(0.,-1.,0.));
#25947=DIRECTION('ref_axis',(-0.959438500558771,0.,0.281918008728669));
#25948=DIRECTION('center_axis',(0.,1.,0.));
#25949=DIRECTION('ref_axis',(-0.959438500551131,0.,0.28191800875467));
#25950=DIRECTION('',(0.,-1.,0.));
#25951=DIRECTION('center_axis',(0.,-1.,0.));
#25952=DIRECTION('ref_axis',(-0.959438500551131,0.,0.28191800875467));
#25953=DIRECTION('center_axis',(-0.470745247127107,0.,0.882269183586982));
#25954=DIRECTION('ref_axis',(0.,1.,0.));
#25955=DIRECTION('',(-0.882269183586788,0.,-0.470745247127471));
#25956=DIRECTION('',(0.,1.,0.));
#25957=DIRECTION('',(0.882269183586788,0.,0.470745247127471));
#25958=DIRECTION('center_axis',(0.528694902398929,0.,-0.848811934516349));
#25959=DIRECTION('ref_axis',(0.,-1.,0.));
#25960=DIRECTION('',(-0.84881193451618,0.,-0.528694902399201));
#25961=DIRECTION('',(0.,-1.,0.));
#25962=DIRECTION('',(0.84881193451618,0.,0.528694902399201));
#25963=DIRECTION('center_axis',(0.634964033941301,0.,-0.772541698292714));
#25964=DIRECTION('ref_axis',(0.,-1.,0.));
#25965=DIRECTION('',(-0.772541698292626,0.,-0.634964033941407));
#25966=DIRECTION('',(0.,-1.,0.));
#25967=DIRECTION('',(0.772541698292626,0.,0.634964033941407));
#25968=DIRECTION('center_axis',(0.813276663802591,0.,-0.581877193327018));
#25969=DIRECTION('ref_axis',(0.,-1.,0.));
#25970=DIRECTION('',(-0.581877193327206,0.,-0.813276663802456));
#25971=DIRECTION('',(0.,-1.,0.));
#25972=DIRECTION('',(0.581877193327206,0.,0.813276663802456));
#25973=DIRECTION('center_axis',(0.882269183586981,0.,-0.470745247127108));
#25974=DIRECTION('ref_axis',(0.,-1.,0.));
#25975=DIRECTION('',(-0.470745247127471,0.,-0.882269183586787));
#25976=DIRECTION('',(0.,-1.,0.));
#25977=DIRECTION('',(0.470745247127471,0.,0.882269183586787));
#25978=DIRECTION('center_axis',(0.,1.,0.));
#25979=DIRECTION('ref_axis',(0.430511096808295,0.,0.902585284349861));
#25980=DIRECTION('center_axis',(0.,-1.,0.));
#25981=DIRECTION('ref_axis',(0.430511096808622,0.,0.902585284349705));
#25982=DIRECTION('',(0.,1.,0.));
#25983=DIRECTION('center_axis',(0.,1.,0.));
#25984=DIRECTION('ref_axis',(0.430511096808622,0.,0.902585284349705));
#25985=DIRECTION('center_axis',(0.,1.,0.));
#25986=DIRECTION('ref_axis',(0.430511096808295,0.,0.902585284349861));
#25987=DIRECTION('center_axis',(0.,1.,0.));
#25988=DIRECTION('ref_axis',(0.430511096808622,0.,0.902585284349705));
#25989=DIRECTION('center_axis',(0.,-1.,0.));
#25990=DIRECTION('ref_axis',(0.430511096808622,0.,0.902585284349705));
#25991=DIRECTION('center_axis',(0.,1.,0.));
#25992=DIRECTION('ref_axis',(1.,0.,0.));
#25993=DIRECTION('',(-0.902585284349658,0.,-0.43051109680872));
#25994=DIRECTION('center_axis',(0.,-1.,0.));
#25995=DIRECTION('ref_axis',(-0.430511096808602,0.,-0.902585284349714));
#25996=DIRECTION('',(0.43051109680872,0.,0.902585284349658));
#25997=DIRECTION('center_axis',(0.,1.,0.));
#25998=DIRECTION('ref_axis',(0.430511096808622,0.,0.902585284349705));
#25999=DIRECTION('center_axis',(0.,1.,0.));
#26000=DIRECTION('ref_axis',(0.430511096808622,0.,0.902585284349705));
#26001=DIRECTION('center_axis',(0.,1.,0.));
#26002=DIRECTION('ref_axis',(0.430511096808622,0.,0.902585284349705));
#26003=DIRECTION('',(-0.683053059422301,0.,-0.730368754817616));
#26004=DIRECTION('center_axis',(0.,1.,0.));
#26005=DIRECTION('ref_axis',(0.430511096808622,0.,0.902585284349705));
#26006=DIRECTION('center_axis',(0.,1.,0.));
#26007=DIRECTION('ref_axis',(0.430511096808295,0.,0.902585284349861));
#26008=DIRECTION('center_axis',(0.,-1.,0.));
#26009=DIRECTION('ref_axis',(0.430511096808622,0.,0.902585284349705));
#26010=DIRECTION('',(0.,-1.,0.));
#26011=DIRECTION('center_axis',(0.,1.,0.));
#26012=DIRECTION('ref_axis',(0.430511096808295,0.,0.902585284349861));
#26013=DIRECTION('',(0.,1.,0.));
#26014=DIRECTION('center_axis',(0.,-1.,0.));
#26015=DIRECTION('ref_axis',(0.430511096808622,0.,0.902585284349705));
#26016=DIRECTION('center_axis',(0.730368754817648,0.,-0.683053059422266));
#26017=DIRECTION('ref_axis',(0.,-1.,0.));
#26018=DIRECTION('',(0.683053059422301,0.,0.730368754817616));
#26019=DIRECTION('center_axis',(0.,1.,0.));
#26020=DIRECTION('ref_axis',(0.430511096808295,0.,0.902585284349861));
#26021=DIRECTION('center_axis',(0.,-1.,0.));
#26022=DIRECTION('ref_axis',(0.430511096808622,0.,0.902585284349705));
#26023=DIRECTION('center_axis',(0.,1.,0.));
#26024=DIRECTION('ref_axis',(-0.430511096808295,0.,-0.902585284349861));
#26025=DIRECTION('',(0.,-1.,0.));
#26026=DIRECTION('center_axis',(0.,1.,0.));
#26027=DIRECTION('ref_axis',(-0.430511096808602,0.,-0.902585284349714));
#26028=DIRECTION('',(0.,1.,0.));
#26029=DIRECTION('center_axis',(0.902585284349861,0.,-0.430511096808294));
#26030=DIRECTION('ref_axis',(0.,-1.,0.));
#26031=DIRECTION('',(-0.43051109680872,0.,-0.902585284349658));
#26032=DIRECTION('center_axis',(0.,1.,0.));
#26033=DIRECTION('ref_axis',(0.430511096808295,0.,0.902585284349861));
#26034=DIRECTION('center_axis',(0.,-1.,0.));
#26035=DIRECTION('ref_axis',(0.430511096808622,0.,0.902585284349705));
#26036=DIRECTION('center_axis',(-0.430511096808294,0.,0.902585284349861));
#26037=DIRECTION('ref_axis',(0.,1.,0.));
#26038=DIRECTION('',(0.902585284349658,0.,0.43051109680872));
#26039=DIRECTION('center_axis',(0.,1.,0.));
#26040=DIRECTION('ref_axis',(1.,0.,0.));
#26041=DIRECTION('axis',(0.,0.,1.));
#26042=DIRECTION('refdir',(1.,0.,0.));
#26043=DIRECTION('center_axis',(0.,1.,0.));
#26044=DIRECTION('ref_axis',(1.,0.,0.));
#26045=DIRECTION('center_axis',(0.,-1.,0.));
#26046=DIRECTION('ref_axis',(-1.,0.,0.));
#26047=DIRECTION('center_axis',(0.,1.,0.));
#26048=DIRECTION('ref_axis',(1.,0.,0.));
#26049=DIRECTION('center_axis',(0.,1.,0.));
#26050=DIRECTION('ref_axis',(1.,0.,0.));
#26051=DIRECTION('',(0.,1.,0.));
#26052=DIRECTION('center_axis',(0.,-1.,0.));
#26053=DIRECTION('ref_axis',(1.,0.,0.));
#26054=DIRECTION('center_axis',(0.,1.,0.));
#26055=DIRECTION('ref_axis',(-1.,0.,0.));
#26056=DIRECTION('center_axis',(0.,1.,0.));
#26057=DIRECTION('ref_axis',(-1.,0.,0.));
#26058=DIRECTION('',(0.,-1.,0.));
#26059=DIRECTION('center_axis',(0.,1.,0.));
#26060=DIRECTION('ref_axis',(1.,0.,0.));
#26061=DIRECTION('axis',(0.,0.,1.));
#26062=DIRECTION('refdir',(1.,0.,0.));
#26063=DIRECTION('center_axis',(1.,5.1420277733694E-16,-1.0522467400333E-14));
#26064=DIRECTION('ref_axis',(-1.0522467400333E-14,1.06077175752244E-14,
-1.));
#26065=DIRECTION('',(-1.00001914094642E-12,1.00002200370999E-12,1.));
#26066=DIRECTION('',(-9.47915311079142E-15,-1.,1.E-14));
#26067=DIRECTION('',(1.00001914094642E-12,-9.99999999998997E-13,-1.));
#26068=DIRECTION('',(-9.47915311079142E-15,-1.,1.E-14));
#26069=DIRECTION('center_axis',(-4.5961454925099E-16,1.,6.61092274672771E-17));
#26070=DIRECTION('ref_axis',(-1.05885766278003E-14,6.61092274672722E-17,
-1.));
#26071=DIRECTION('',(1.,-9.54038545074888E-15,9.9999999999998E-15));
#26072=DIRECTION('',(-9.56631913100564E-15,9.99999999999985E-15,1.));
#26073=DIRECTION('',(-1.,9.54038545074888E-15,-9.9999999999998E-15));
#26074=DIRECTION('center_axis',(-1.0522467400333E-14,6.93088260946523E-29,
-1.));
#26075=DIRECTION('ref_axis',(1.,-6.62426369448742E-15,-1.0522467400333E-14));
#26076=DIRECTION('',(-9.47915311079142E-15,-1.,1.E-14));
#26077=DIRECTION('center_axis',(-1.99999999991998E-11,2.E-11,1.));
#26078=DIRECTION('ref_axis',(-1.99995712428458E-11,-1.,1.99999999996E-11));
#26079=DIRECTION('',(1.,-9.99466108488984E-13,9.99906900405741E-13));
#26080=DIRECTION('',(9.99479153109778E-13,1.,-1.00002200371E-12));
#26081=DIRECTION('',(-1.,9.99485333130104E-13,-1.00005108521413E-12));
#26082=DIRECTION('center_axis',(0.,-4.29362650667545E-31,1.));
#26083=DIRECTION('ref_axis',(4.28756753891971E-16,-1.,-4.29362650667545E-31));
#26084=DIRECTION('',(-9.99999999999976E-15,-1.04336808689941E-14,1.));
#26085=DIRECTION('',(-9.56631913100564E-15,9.99999999999985E-15,1.));
#26086=DIRECTION('center_axis',(-1.99999999991998E-11,2.E-11,1.));
#26087=DIRECTION('ref_axis',(-1.99995712428458E-11,-1.,1.99999999996E-11));
#26088=DIRECTION('center_axis',(0.,3.71824206197546E-31,1.));
#26089=DIRECTION('ref_axis',(1.,3.89820370584558E-15,-1.44944649852236E-45));
#26090=DIRECTION('',(-9.47915311079142E-15,-1.,1.E-14));
#26091=DIRECTION('',(1.,-9.99466108488984E-13,9.99906900405741E-13));
#26092=DIRECTION('',(-9.99479153109778E-13,-1.,1.00002200371E-12));
#26093=DIRECTION('',(1.,-9.99466108488984E-13,9.99906900405741E-13));
#26094=DIRECTION('center_axis',(1.,5.2084688920845E-16,-1.0522467400333E-14));
#26095=DIRECTION('ref_axis',(-1.0522467400333E-14,1.01548957588061E-14,
-1.));
#26096=DIRECTION('center_axis',(5.33891510011771E-16,-1.,2.20037109950003E-17));
#26097=DIRECTION('ref_axis',(-1.,-5.33891510011771E-16,1.0522467400333E-14));
#26098=DIRECTION('',(9.99999999998993E-13,-1.00002200370999E-12,-1.));
#26099=DIRECTION('center_axis',(-5.3389151001177E-16,1.,6.61092274672778E-17));
#26100=DIRECTION('ref_axis',(-1.06105803387953E-14,6.61092274672721E-17,
-1.));
#26101=DIRECTION('',(-9.99999999998993E-13,1.00002200370999E-12,1.));
#26102=DIRECTION('center_axis',(1.,5.3389151001188E-16,-1.0522467400333E-14));
#26103=DIRECTION('ref_axis',(-1.0522467400333E-14,1.04954770345521E-14,
-1.));
#26104=DIRECTION('axis',(0.,0.,1.));
#26105=DIRECTION('refdir',(1.,0.,0.));
#26106=DIRECTION('center_axis',(6.65798752924967E-17,-1.,1.71022579061586E-31));
#26107=DIRECTION('ref_axis',(-0.345824623417469,-2.30249603002096E-17,0.938299168622762));
#26108=DIRECTION('',(6.65798752924967E-17,-1.,1.71022579061586E-31));
#26109=DIRECTION('center_axis',(6.65798752924967E-17,-1.,1.71022579061586E-31));
#26110=DIRECTION('ref_axis',(-0.345824623433441,-2.3024960301273E-17,0.938299168616875));
#26111=DIRECTION('',(-6.65798752924967E-17,1.,-1.71022579061586E-31));
#26112=DIRECTION('center_axis',(-6.65798752924967E-17,1.,-1.71022579061586E-31));
#26113=DIRECTION('ref_axis',(-0.345824623433441,-2.3024960301273E-17,0.938299168616875));
#26114=DIRECTION('center_axis',(6.65798752924967E-17,-1.,1.71022579061586E-31));
#26115=DIRECTION('ref_axis',(-0.473045086880378,-3.14952828922237E-17,0.881038220384528));
#26116=DIRECTION('',(6.65798752924967E-17,-1.,1.71022579061586E-31));
#26117=DIRECTION('center_axis',(6.65798752924967E-17,-1.,1.71022579061586E-31));
#26118=DIRECTION('ref_axis',(-0.473045086892459,-3.1495282893028E-17,0.881038220378041));
#26119=DIRECTION('',(-6.65798752924967E-17,1.,-1.71022579061586E-31));
#26120=DIRECTION('center_axis',(-6.65798752924967E-17,1.,-1.71022579061586E-31));
#26121=DIRECTION('ref_axis',(-0.473045086892459,-3.1495282893028E-17,0.881038220378041));
#26122=DIRECTION('center_axis',(6.65798752924967E-17,-1.,1.71022579061586E-31));
#26123=DIRECTION('ref_axis',(-0.591058265807973,-3.93525856280941E-17,0.80662886535263));
#26124=DIRECTION('',(6.65798752924967E-17,-1.,1.71022579061586E-31));
#26125=DIRECTION('center_axis',(6.65798752924967E-17,-1.,1.71022579061586E-31));
#26126=DIRECTION('ref_axis',(-0.591058265816149,-3.93525856286384E-17,0.806628865346639));
#26127=DIRECTION('',(-6.65798752924967E-17,1.,-1.71022579061586E-31));
#26128=DIRECTION('center_axis',(-6.65798752924967E-17,1.,-1.71022579061586E-31));
#26129=DIRECTION('ref_axis',(-0.591058265816149,-3.93525856286384E-17,0.806628865346639));
#26130=DIRECTION('center_axis',(6.65798752924967E-17,-1.,1.71022579061586E-31));
#26131=DIRECTION('ref_axis',(-0.697567167910428,-4.64439350476163E-17,0.716519396983379));
#26132=DIRECTION('',(6.65798752924967E-17,-1.,1.71022579061586E-31));
#26133=DIRECTION('center_axis',(6.65798752924967E-17,-1.,1.71022579061586E-31));
#26134=DIRECTION('ref_axis',(-0.697567167914987,-4.64439350479198E-17,0.716519396978941));
#26135=DIRECTION('',(-6.65798752924967E-17,1.,-1.71022579061586E-31));
#26136=DIRECTION('center_axis',(-6.65798752924967E-17,1.,-1.71022579061586E-31));
#26137=DIRECTION('ref_axis',(-0.697567167914987,-4.64439350479198E-17,0.716519396978941));
#26138=DIRECTION('center_axis',(6.65798752924967E-17,-1.,1.71022579061586E-31));
#26139=DIRECTION('ref_axis',(-0.790498718560399,-5.26313061006297E-17,0.61246369358058));
#26140=DIRECTION('',(6.65798752924967E-17,-1.,1.71022579061586E-31));
#26141=DIRECTION('center_axis',(6.65798752924967E-17,-1.,1.71022579061586E-31));
#26142=DIRECTION('ref_axis',(-0.790498718561909,-5.26313061007302E-17,0.612463693578632));
#26143=DIRECTION('',(-6.65798752924967E-17,1.,-1.71022579061586E-31));
#26144=DIRECTION('center_axis',(-6.65798752924967E-17,1.,-1.71022579061586E-31));
#26145=DIRECTION('ref_axis',(-0.790498718561909,-5.26313061007302E-17,0.612463693578632));
#26146=DIRECTION('center_axis',(6.65798752924967E-17,-1.,1.71022579061586E-31));
#26147=DIRECTION('ref_axis',(-0.868044110832557,-5.77942686476178E-17,0.496487081049362));
#26148=DIRECTION('',(6.65798752924967E-17,-1.,1.71022579061586E-31));
#26149=DIRECTION('center_axis',(6.65798752924967E-17,-1.,1.71022579061586E-31));
#26150=DIRECTION('ref_axis',(-0.868044110831822,-5.77942686475688E-17,0.496487081050647));
#26151=DIRECTION('',(-6.65798752924967E-17,1.,-1.71022579061586E-31));
#26152=DIRECTION('center_axis',(-6.65798752924967E-17,1.,-1.71022579061586E-31));
#26153=DIRECTION('ref_axis',(-0.868044110831822,-5.77942686475688E-17,0.496487081050647));
#26154=DIRECTION('center_axis',(6.65798752924967E-17,-1.,1.71022579061586E-31));
#26155=DIRECTION('ref_axis',(-0.928694011872901,-6.18323314953861E-17,0.370846912231201));
#26156=DIRECTION('',(6.65798752924967E-17,-1.,1.71022579061586E-31));
#26157=DIRECTION('center_axis',(6.65798752924967E-17,-1.,1.71022579061586E-31));
#26158=DIRECTION('ref_axis',(-0.9286940118709,-6.18323314952529E-17,0.370846912236213));
#26159=DIRECTION('',(-6.65798752924967E-17,1.,-1.71022579061586E-31));
#26160=DIRECTION('center_axis',(-6.65798752924967E-17,1.,-1.71022579061586E-31));
#26161=DIRECTION('ref_axis',(-0.9286940118709,-6.18323314952529E-17,0.370846912236213));
#26162=DIRECTION('center_axis',(6.65798752924967E-17,-1.,1.71022579061586E-31));
#26163=DIRECTION('ref_axis',(-0.97126794034592,-6.46668983438314E-17,0.237988630098571));
#26164=DIRECTION('',(6.65798752924967E-17,-1.,1.71022579061586E-31));
#26165=DIRECTION('center_axis',(6.65798752924967E-17,-1.,1.71022579061586E-31));
#26166=DIRECTION('ref_axis',(-0.971267940343728,-6.46668983436855E-17,0.237988630107515));
#26167=DIRECTION('',(-6.65798752924967E-17,1.,-1.71022579061586E-31));
#26168=DIRECTION('center_axis',(-6.65798752924967E-17,1.,-1.71022579061586E-31));
#26169=DIRECTION('ref_axis',(-0.971267940343728,-6.46668983436855E-17,0.237988630107515));
#26170=DIRECTION('center_axis',(6.65798752924967E-17,-1.,1.71022579061586E-31));
#26171=DIRECTION('ref_axis',(-0.994937243161013,-6.62427975735207E-17,0.100498169989126));
#26172=DIRECTION('',(6.65798752924967E-17,-1.,1.71022579061586E-31));
#26173=DIRECTION('center_axis',(6.65798752924967E-17,-1.,1.71022579061586E-31));
#26174=DIRECTION('ref_axis',(-0.994937243159722,-6.62427975734348E-17,0.100498170001902));
#26175=DIRECTION('',(-6.65798752924967E-17,1.,-1.71022579061586E-31));
#26176=DIRECTION('center_axis',(-6.65798752924967E-17,1.,-1.71022579061586E-31));
#26177=DIRECTION('ref_axis',(-0.994937243159722,-6.62427975734348E-17,0.100498170001902));
#26178=DIRECTION('center_axis',(6.65798752924967E-17,-1.,1.71022579061586E-31));
#26179=DIRECTION('ref_axis',(-0.999241224262317,-6.65293560985068E-17,-0.0389483726841831));
#26180=DIRECTION('',(6.65798752924967E-17,-1.,1.71022579061586E-31));
#26181=DIRECTION('center_axis',(6.65798752924967E-17,-1.,1.71022579061586E-31));
#26182=DIRECTION('ref_axis',(-0.999241224262949,-6.65293560985489E-17,-0.038948372667972));
#26183=DIRECTION('',(-6.65798752924967E-17,1.,-1.71022579061586E-31));
#26184=DIRECTION('center_axis',(-6.65798752924967E-17,1.,-1.71022579061586E-31));
#26185=DIRECTION('ref_axis',(-0.999241224262949,-6.65293560985489E-17,-0.038948372667972));
#26186=DIRECTION('center_axis',(6.65798752924967E-17,-1.,1.71022579061586E-31));
#26187=DIRECTION('ref_axis',(-0.984096111553401,-6.55209963830564E-17,-0.177636829586311));
#26188=DIRECTION('',(6.65798752924967E-17,-1.,1.71022579061586E-31));
#26189=DIRECTION('center_axis',(6.65798752924967E-17,-1.,1.71022579061586E-31));
#26190=DIRECTION('ref_axis',(-0.984096111556828,-6.55209963832845E-17,-0.177636829567328));
#26191=DIRECTION('',(-6.65798752924967E-17,1.,-1.71022579061586E-31));
#26192=DIRECTION('center_axis',(-6.65798752924967E-17,1.,-1.71022579061586E-31));
#26193=DIRECTION('ref_axis',(-0.984096111556828,-6.55209963832845E-17,-0.177636829567328));
#26194=DIRECTION('center_axis',(6.65798752924967E-17,-1.,1.71022579061586E-31));
#26195=DIRECTION('ref_axis',(-0.949796687425834,-6.32373450020385E-17,-0.312867787659441));
#26196=DIRECTION('',(6.65798752924967E-17,-1.,1.71022579061586E-31));
#26197=DIRECTION('center_axis',(6.65798752924967E-17,-1.,1.71022579061586E-31));
#26198=DIRECTION('ref_axis',(-0.949796687420265,-6.32373450016678E-17,-0.312867787676347));
#26199=DIRECTION('',(-6.65798752924967E-17,1.,-1.71022579061586E-31));
#26200=DIRECTION('center_axis',(-6.65798752924967E-17,1.,-1.71022579061586E-31));
#26201=DIRECTION('ref_axis',(-0.949796687420265,-6.32373450016678E-17,-0.312867787676347));
#26202=DIRECTION('center_axis',(6.65798752924967E-17,-1.,1.71022579061586E-31));
#26203=DIRECTION('ref_axis',(-0.897010551155241,-5.97228506319698E-17,-0.442009130127614));
#26204=DIRECTION('',(6.65798752924967E-17,-1.,1.71022579061586E-31));
#26205=DIRECTION('center_axis',(6.65798752924967E-17,-1.,1.71022579061586E-31));
#26206=DIRECTION('ref_axis',(-0.897010551148803,-5.97228506315411E-17,-0.442009130140681));
#26207=DIRECTION('',(-6.65798752924967E-17,1.,-1.71022579061586E-31));
#26208=DIRECTION('center_axis',(-6.65798752924967E-17,1.,-1.71022579061586E-31));
#26209=DIRECTION('ref_axis',(-0.897010551148803,-5.97228506315411E-17,-0.442009130140681));
#26210=DIRECTION('center_axis',(6.65798752924967E-17,-1.,1.71022579061586E-31));
#26211=DIRECTION('ref_axis',(-0.826765124840791,-5.50459189080855E-17,-0.562547267655786));
#26212=DIRECTION('',(6.65798752924967E-17,-1.,1.71022579061586E-31));
#26213=DIRECTION('center_axis',(6.65798752924967E-17,-1.,1.71022579061586E-31));
#26214=DIRECTION('ref_axis',(-0.826765124834574,-5.50459189076715E-17,-0.562547267664923));
#26215=DIRECTION('',(-6.65798752924967E-17,1.,-1.71022579061586E-31));
#26216=DIRECTION('center_axis',(-6.65798752924967E-17,1.,-1.71022579061586E-31));
#26217=DIRECTION('ref_axis',(-0.826765124834574,-5.50459189076715E-17,-0.562547267664923));
#26218=DIRECTION('center_axis',(6.65798752924967E-17,-1.,1.71022579061586E-31));
#26219=DIRECTION('ref_axis',(-0.740427655802706,-4.929758098646E-17,-0.672136062507071));
#26220=DIRECTION('',(6.65798752924967E-17,-1.,1.71022579061586E-31));
#26221=DIRECTION('center_axis',(6.65798752924967E-17,-1.,1.71022579061586E-31));
#26222=DIRECTION('ref_axis',(-0.740427655797785,-4.92975809861323E-17,-0.672136062512493));
#26223=DIRECTION('',(-6.65798752924967E-17,1.,-1.71022579061586E-31));
#26224=DIRECTION('center_axis',(-6.65798752924967E-17,1.,-1.71022579061586E-31));
#26225=DIRECTION('ref_axis',(-0.740427655797785,-4.92975809861323E-17,-0.672136062512493));
#26226=DIRECTION('center_axis',(6.65798752924967E-17,-1.,1.71022579061586E-31));
#26227=DIRECTION('ref_axis',(-0.639678604668397,-4.25897217261003E-17,-0.768642493445095));
#26228=DIRECTION('',(6.65798752924967E-17,-1.,1.71022579061586E-31));
#26229=DIRECTION('center_axis',(6.65798752924967E-17,-1.,1.71022579061586E-31));
#26230=DIRECTION('ref_axis',(-0.639678604665747,-4.25897217259239E-17,-0.7686424934473));
#26231=DIRECTION('',(-6.65798752924967E-17,1.,-1.71022579061586E-31));
#26232=DIRECTION('center_axis',(-6.65798752924967E-17,1.,-1.71022579061586E-31));
#26233=DIRECTION('ref_axis',(-0.639678604665747,-4.25897217259239E-17,-0.7686424934473));
#26234=DIRECTION('center_axis',(6.65798752924967E-17,-1.,1.71022579061586E-31));
#26235=DIRECTION('ref_axis',(-0.526478937117844,-3.50529019774324E-17,-0.850188172566088));
#26236=DIRECTION('',(6.65798752924967E-17,-1.,1.71022579061586E-31));
#26237=DIRECTION('center_axis',(6.65798752924967E-17,-1.,1.71022579061586E-31));
#26238=DIRECTION('ref_axis',(-0.526478937118264,-3.50529019774604E-17,-0.850188172565828));
#26239=DIRECTION('',(-6.65798752924967E-17,1.,-1.71022579061586E-31));
#26240=DIRECTION('center_axis',(-6.65798752924967E-17,1.,-1.71022579061586E-31));
#26241=DIRECTION('ref_axis',(-0.526478937118264,-3.50529019774604E-17,-0.850188172565828));
#26242=DIRECTION('center_axis',(6.65798752924967E-17,-1.,1.71022579061586E-31));
#26243=DIRECTION('ref_axis',(-0.403031955917209,-2.6833817363859E-17,-0.915185905982795));
#26244=DIRECTION('',(6.65798752924967E-17,-1.,1.71022579061586E-31));
#26245=DIRECTION('center_axis',(6.65798752924967E-17,-1.,1.71022579061586E-31));
#26246=DIRECTION('ref_axis',(-0.403031955921259,-2.68338173641286E-17,-0.915185905981011));
#26247=DIRECTION('',(-6.65798752924967E-17,1.,-1.71022579061586E-31));
#26248=DIRECTION('center_axis',(-6.65798752924967E-17,1.,-1.71022579061586E-31));
#26249=DIRECTION('ref_axis',(-0.403031955921259,-2.68338173641286E-17,-0.915185905981011));
#26250=DIRECTION('center_axis',(6.65798752924967E-17,-1.,1.71022579061586E-31));
#26251=DIRECTION('ref_axis',(-0.2717404161367,-1.80924430183128E-17,-0.962370586748085));
#26252=DIRECTION('',(6.65798752924967E-17,-1.,1.71022579061586E-31));
#26253=DIRECTION('center_axis',(6.65798752924967E-17,-1.,1.71022579061586E-31));
#26254=DIRECTION('ref_axis',(-0.271740416144659,-1.80924430188427E-17,-0.962370586745838));
#26255=DIRECTION('',(-6.65798752924967E-17,1.,-1.71022579061586E-31));
#26256=DIRECTION('center_axis',(-6.65798752924967E-17,1.,-1.71022579061586E-31));
#26257=DIRECTION('ref_axis',(-0.271740416144659,-1.80924430188427E-17,-0.962370586745838));
#26258=DIRECTION('center_axis',(6.65798752924967E-17,-1.,1.71022579061586E-31));
#26259=DIRECTION('ref_axis',(-0.135159758256232,-8.9989198492641E-18,-0.990823818722641));
#26260=DIRECTION('',(6.65798752924967E-17,-1.,1.71022579061586E-31));
#26261=DIRECTION('center_axis',(6.65798752924967E-17,-1.,1.71022579061586E-31));
#26262=DIRECTION('ref_axis',(-0.135159758268076,-8.99891985005266E-18,-0.990823818721025));
#26263=DIRECTION('',(-6.65798752924967E-17,1.,-1.71022579061586E-31));
#26264=DIRECTION('center_axis',(-6.65798752924967E-17,1.,-1.71022579061586E-31));
#26265=DIRECTION('ref_axis',(-0.135159758268076,-8.99891985005266E-18,-0.990823818721025));
#26266=DIRECTION('center_axis',(6.65798752924967E-17,-1.,1.71022579061586E-31));
#26267=DIRECTION('ref_axis',(0.00405163057674682,2.69757058530899E-19,-0.99999179211115));
#26268=DIRECTION('',(6.65798752924967E-17,-1.,1.71022579061586E-31));
#26269=DIRECTION('center_axis',(6.65798752924967E-17,-1.,1.71022579061586E-31));
#26270=DIRECTION('ref_axis',(0.00405163056134247,2.69757057505279E-19,-0.999991792111212));
#26271=DIRECTION('',(-6.65798752924967E-17,1.,-1.71022579061586E-31));
#26272=DIRECTION('center_axis',(-6.65798752924967E-17,1.,-1.71022579061586E-31));
#26273=DIRECTION('ref_axis',(0.00405163056134247,2.69757057505279E-19,-0.999991792111212));
#26274=DIRECTION('center_axis',(6.65798752924967E-17,-1.,1.71022579061586E-31));
#26275=DIRECTION('ref_axis',(0.143184159029212,9.53318345202578E-18,-0.98969606274002));
#26276=DIRECTION('',(6.65798752924967E-17,-1.,1.71022579061586E-31));
#26277=DIRECTION('center_axis',(6.65798752924967E-17,-1.,1.71022579061586E-31));
#26278=DIRECTION('ref_axis',(0.143184159010847,9.53318345080304E-18,-0.989696062742677));
#26279=DIRECTION('',(-6.65798752924967E-17,1.,-1.71022579061586E-31));
#26280=DIRECTION('center_axis',(-6.65798752924967E-17,1.,-1.71022579061586E-31));
#26281=DIRECTION('ref_axis',(0.143184159010847,9.53318345080304E-18,-0.989696062742677));
#26282=DIRECTION('center_axis',(6.65798752924967E-17,-1.,1.71022579061586E-31));
#26283=DIRECTION('ref_axis',(0.27952977069574,1.86110572734624E-17,-0.960137025270241));
#26284=DIRECTION('',(6.65798752924967E-17,-1.,1.71022579061586E-31));
#26285=DIRECTION('center_axis',(6.65798752924967E-17,-1.,1.71022579061586E-31));
#26286=DIRECTION('ref_axis',(0.279529770713557,1.86110572746487E-17,-0.960137025265054));
#26287=DIRECTION('',(-6.65798752924967E-17,1.,-1.71022579061586E-31));
#26288=DIRECTION('center_axis',(-6.65798752924967E-17,1.,-1.71022579061586E-31));
#26289=DIRECTION('ref_axis',(0.279529770713557,1.86110572746487E-17,-0.960137025265054));
#26290=DIRECTION('center_axis',(6.65798752924967E-17,-1.,1.71022579061586E-31));
#26291=DIRECTION('ref_axis',(0.410434653336076,2.73266880348349E-17,-0.911890012743256));
#26292=DIRECTION('',(6.65798752924967E-17,-1.,1.71022579061586E-31));
#26293=DIRECTION('center_axis',(6.65798752924967E-17,-1.,1.71022579061586E-31));
#26294=DIRECTION('ref_axis',(0.410434653350123,2.73266880357702E-17,-0.911890012736933));
#26295=DIRECTION('',(-6.65798752924967E-17,1.,-1.71022579061586E-31));
#26296=DIRECTION('center_axis',(-6.65798752924967E-17,1.,-1.71022579061586E-31));
#26297=DIRECTION('ref_axis',(0.410434653350123,2.73266880357702E-17,-0.911890012736933));
#26298=DIRECTION('center_axis',(6.65798752924967E-17,-1.,1.71022579061586E-31));
#26299=DIRECTION('ref_axis',(0.533350892311725,3.55104358972563E-17,-0.845894098377738));
#26300=DIRECTION('',(6.65798752924967E-17,-1.,1.71022579061586E-31));
#26301=DIRECTION('center_axis',(6.65798752924967E-17,-1.,1.71022579061586E-31));
#26302=DIRECTION('ref_axis',(0.533350892321836,3.55104358979295E-17,-0.845894098371363));
#26303=DIRECTION('',(-6.65798752924967E-17,1.,-1.71022579061586E-31));
#26304=DIRECTION('center_axis',(-6.65798752924967E-17,1.,-1.71022579061586E-31));
#26305=DIRECTION('ref_axis',(0.533350892321836,3.55104358979295E-17,-0.845894098371363));
#26306=DIRECTION('center_axis',(6.65798752924967E-17,-1.,1.71022579061586E-31));
#26307=DIRECTION('ref_axis',(0.645886062846174,4.30030135174598E-17,-0.763433817577574));
#26308=DIRECTION('',(6.65798752924967E-17,-1.,1.71022579061586E-31));
#26309=DIRECTION('center_axis',(6.65798752924967E-17,-1.,1.71022579061586E-31));
#26310=DIRECTION('ref_axis',(0.645886062852486,4.30030135178801E-17,-0.763433817572233));
#26311=DIRECTION('',(-6.65798752924967E-17,1.,-1.71022579061586E-31));
#26312=DIRECTION('center_axis',(-6.65798752924967E-17,1.,-1.71022579061586E-31));
#26313=DIRECTION('ref_axis',(0.645886062852486,4.30030135178801E-17,-0.763433817572233));
#26314=DIRECTION('center_axis',(6.65798752924967E-17,-1.,1.71022579061586E-31));
#26315=DIRECTION('ref_axis',(0.745849795851828,4.96585863947487E-17,-0.666114165911359));
#26316=DIRECTION('',(6.65798752924967E-17,-1.,1.71022579061586E-31));
#26317=DIRECTION('center_axis',(6.65798752924967E-17,-1.,1.71022579061586E-31));
#26318=DIRECTION('ref_axis',(0.745849795854776,4.9658586394945E-17,-0.66611416590806));
#26319=DIRECTION('',(-6.65798752924967E-17,1.,-1.71022579061586E-31));
#26320=DIRECTION('center_axis',(-6.65798752924967E-17,1.,-1.71022579061586E-31));
#26321=DIRECTION('ref_axis',(0.745849795854776,4.9658586394945E-17,-0.66611416590806));
#26322=DIRECTION('center_axis',(6.65798752924967E-17,-1.,1.71022579061586E-31));
#26323=DIRECTION('ref_axis',(0.831296410972796,5.53476113736688E-17,-0.555829359699313));
#26324=DIRECTION('',(6.65798752924967E-17,-1.,1.71022579061586E-31));
#26325=DIRECTION('center_axis',(6.65798752924967E-17,-1.,1.71022579061586E-31));
#26326=DIRECTION('ref_axis',(0.83129641097307,5.5347611373687E-17,-0.555829359698903));
#26327=DIRECTION('',(-6.65798752924967E-17,1.,-1.71022579061586E-31));
#26328=DIRECTION('center_axis',(-6.65798752924967E-17,1.,-1.71022579061586E-31));
#26329=DIRECTION('ref_axis',(0.83129641097307,5.5347611373687E-17,-0.555829359698903));
#26330=DIRECTION('center_axis',(6.65798752924967E-17,-1.,1.71022579061586E-31));
#26331=DIRECTION('ref_axis',(0.900562787039831,5.99593580541751E-17,-0.434725967247245));
#26332=DIRECTION('',(6.65798752924967E-17,-1.,1.71022579061586E-31));
#26333=DIRECTION('center_axis',(6.65798752924967E-17,-1.,1.71022579061586E-31));
#26334=DIRECTION('ref_axis',(0.900562787038332,5.99593580540753E-17,-0.434725967250349));
#26335=DIRECTION('',(-6.65798752924967E-17,1.,-1.71022579061586E-31));
#26336=DIRECTION('center_axis',(-6.65798752924967E-17,1.,-1.71022579061586E-31));
#26337=DIRECTION('ref_axis',(0.900562787038332,5.99593580540753E-17,-0.434725967250349));
#26338=DIRECTION('center_axis',(6.65798752924967E-17,-1.,1.71022579061586E-31));
#26339=DIRECTION('ref_axis',(0.952300732832122,6.34040640329159E-17,-0.305161128336168));
#26340=DIRECTION('',(6.65798752924967E-17,-1.,1.71022579061586E-31));
#26341=DIRECTION('center_axis',(6.65798752924967E-17,-1.,1.71022579061586E-31));
#26342=DIRECTION('ref_axis',(0.952300732829888,6.34040640327671E-17,-0.30516112834314));
#26343=DIRECTION('',(-6.65798752924967E-17,1.,-1.71022579061586E-31));
#26344=DIRECTION('center_axis',(-6.65798752924967E-17,1.,-1.71022579061586E-31));
#26345=DIRECTION('ref_axis',(0.952300732829888,6.34040640327671E-17,-0.30516112834314));
#26346=DIRECTION('center_axis',(6.65798752924967E-17,-1.,1.71022579061586E-31));
#26347=DIRECTION('ref_axis',(0.985503228085865,6.56146820263098E-17,-0.169656675177667));
#26348=DIRECTION('',(6.65798752924967E-17,-1.,1.71022579061586E-31));
#26349=DIRECTION('center_axis',(6.65798752924967E-17,-1.,1.71022579061586E-31));
#26350=DIRECTION('ref_axis',(0.985503228083989,6.56146820261849E-17,-0.169656675188558));
#26351=DIRECTION('',(-6.65798752924967E-17,1.,-1.71022579061586E-31));
#26352=DIRECTION('center_axis',(-6.65798752924967E-17,1.,-1.71022579061586E-31));
#26353=DIRECTION('ref_axis',(0.985503228083989,6.56146820261849E-17,-0.169656675188558));
#26354=DIRECTION('center_axis',(6.65798752924967E-17,-1.,1.71022579061586E-31));
#26355=DIRECTION('ref_axis',(0.999524023998223,6.65481848696562E-17,-0.0308500478184399));
#26356=DIRECTION('',(6.65798752924967E-17,-1.,1.71022579061586E-31));
#26357=DIRECTION('center_axis',(6.65798752924967E-17,-1.,1.71022579061586E-31));
#26358=DIRECTION('ref_axis',(0.999524023997774,6.65481848696262E-17,-0.0308500478330001));
#26359=DIRECTION('',(-6.65798752924967E-17,1.,-1.71022579061586E-31));
#26360=DIRECTION('center_axis',(-6.65798752924967E-17,1.,-1.71022579061586E-31));
#26361=DIRECTION('ref_axis',(0.999524023997774,6.65481848696262E-17,-0.0308500478330001));
#26362=DIRECTION('center_axis',(6.65798752924967E-17,-1.,1.71022579061586E-31));
#26363=DIRECTION('ref_axis',(0.994090221725182,6.6186402991953E-17,0.108557040630164));
#26364=DIRECTION('',(6.65798752924967E-17,-1.,1.71022579061586E-31));
#26365=DIRECTION('center_axis',(6.65798752924967E-17,-1.,1.71022579061586E-31));
#26366=DIRECTION('ref_axis',(0.994090221727114,6.61864029920817E-17,0.108557040612469));
#26367=DIRECTION('',(-6.65798752924967E-17,1.,-1.71022579061586E-31));
#26368=DIRECTION('center_axis',(-6.65798752924967E-17,1.,-1.71022579061586E-31));
#26369=DIRECTION('ref_axis',(0.994090221727114,6.61864029920817E-17,0.108557040612469));
#26370=DIRECTION('center_axis',(6.65798752924967E-17,-1.,1.71022579061586E-31));
#26371=DIRECTION('ref_axis',(0.969307584047127,6.4536378065929E-17,0.245851189764706));
#26372=DIRECTION('',(6.65798752924967E-17,-1.,1.71022579061586E-31));
#26373=DIRECTION('center_axis',(6.65798752924967E-17,-1.,1.71022579061586E-31));
#26374=DIRECTION('ref_axis',(0.969307584042385,6.45363780656133E-17,0.245851189783404));
#26375=DIRECTION('',(-6.65798752924967E-17,1.,-1.71022579061586E-31));
#26376=DIRECTION('center_axis',(-6.65798752924967E-17,1.,-1.71022579061586E-31));
#26377=DIRECTION('ref_axis',(0.969307584042385,6.45363780656133E-17,0.245851189783404));
#26378=DIRECTION('center_axis',(6.65798752924967E-17,-1.,1.71022579061586E-31));
#26379=DIRECTION('ref_axis',(0.925658476816631,6.16302259498938E-17,0.37836012514206));
#26380=DIRECTION('',(6.65798752924967E-17,-1.,1.71022579061586E-31));
#26381=DIRECTION('center_axis',(6.65798752924967E-17,-1.,1.71022579061586E-31));
#26382=DIRECTION('ref_axis',(0.925658476810492,6.16302259494851E-17,0.378360125157078));
#26383=DIRECTION('',(-6.65798752924967E-17,1.,-1.71022579061586E-31));
#26384=DIRECTION('center_axis',(-6.65798752924967E-17,1.,-1.71022579061586E-31));
#26385=DIRECTION('ref_axis',(0.925658476810492,6.16302259494851E-17,0.378360125157078));
#26386=DIRECTION('center_axis',(6.65798752924967E-17,-1.,1.71022579061586E-31));
#26387=DIRECTION('ref_axis',(0.86399248025581,5.75245115890868E-17,0.503504711061788));
#26388=DIRECTION('',(6.65798752924967E-17,-1.,1.71022579061586E-31));
#26389=DIRECTION('center_axis',(6.65798752924967E-17,-1.,1.71022579061586E-31));
#26390=DIRECTION('ref_axis',(0.863992480249344,5.75245115886563E-17,0.503504711072882));
#26391=DIRECTION('',(-6.65798752924967E-17,1.,-1.71022579061586E-31));
#26392=DIRECTION('center_axis',(-6.65798752924967E-17,1.,-1.71022579061586E-31));
#26393=DIRECTION('ref_axis',(0.863992480249344,5.75245115886563E-17,0.503504711072882));
#26394=DIRECTION('center_axis',(6.65798752924967E-17,-1.,1.71022579061586E-31));
#26395=DIRECTION('ref_axis',(0.785509852843689,5.22991480433604E-17,0.618849150508818));
#26396=DIRECTION('',(6.65798752924967E-17,-1.,1.71022579061586E-31));
#26397=DIRECTION('center_axis',(6.65798752924967E-17,-1.,1.71022579061586E-31));
#26398=DIRECTION('ref_axis',(0.78550985283799,5.22991480429809E-17,0.618849150516052));
#26399=DIRECTION('',(-6.65798752924967E-17,1.,-1.71022579061586E-31));
#26400=DIRECTION('center_axis',(-6.65798752924967E-17,1.,-1.71022579061586E-31));
#26401=DIRECTION('ref_axis',(0.78550985283799,5.22991480429809E-17,0.618849150516052));
#26402=DIRECTION('center_axis',(6.65798752924967E-17,-1.,1.71022579061586E-31));
#26403=DIRECTION('ref_axis',(0.691738169650181,4.60558410703691E-17,0.72214839517167));
#26404=DIRECTION('',(6.65798752924967E-17,-1.,1.71022579061586E-31));
#26405=DIRECTION('center_axis',(6.65798752924967E-17,-1.,1.71022579061586E-31));
#26406=DIRECTION('ref_axis',(0.691738169646283,4.60558410701096E-17,0.722148395175403));
#26407=DIRECTION('',(-6.65798752924967E-17,1.,-1.71022579061586E-31));
#26408=DIRECTION('center_axis',(-6.65798752924967E-17,1.,-1.71022579061586E-31));
#26409=DIRECTION('ref_axis',(0.691738169646283,4.60558410701096E-17,0.722148395175403));
#26410=DIRECTION('center_axis',(6.65798752924967E-17,-1.,1.71022579061586E-31));
#26411=DIRECTION('ref_axis',(0.584502589824937,3.89161095386858E-17,0.811391842754129));
#26412=DIRECTION('',(6.65798752924967E-17,-1.,1.71022579061586E-31));
#26413=DIRECTION('center_axis',(6.65798752924967E-17,-1.,1.71022579061586E-31));
#26414=DIRECTION('ref_axis',(0.584502589823736,3.89161095386059E-17,0.811391842754994));
#26415=DIRECTION('',(-6.65798752924967E-17,1.,-1.71022579061586E-31));
#26416=DIRECTION('center_axis',(-6.65798752924967E-17,1.,-1.71022579061586E-31));
#26417=DIRECTION('ref_axis',(0.584502589823736,3.89161095386059E-17,0.811391842754994));
#26418=DIRECTION('center_axis',(6.65798752924967E-17,-1.,1.71022579061586E-31));
#26419=DIRECTION('ref_axis',(0.465890331950592,3.10189202012505E-17,0.884842471061921));
#26420=DIRECTION('',(6.65798752924967E-17,-1.,1.71022579061586E-31));
#26421=DIRECTION('center_axis',(6.65798752924967E-17,-1.,1.71022579061586E-31));
#26422=DIRECTION('ref_axis',(0.465890331952774,3.10189202013957E-17,0.884842471060773));
#26423=DIRECTION('',(-6.65798752924967E-17,1.,-1.71022579061586E-31));
#26424=DIRECTION('center_axis',(-6.65798752924967E-17,1.,-1.71022579061586E-31));
#26425=DIRECTION('ref_axis',(0.465890331952774,3.10189202013957E-17,0.884842471060773));
#26426=DIRECTION('center_axis',(6.65798752924967E-17,-1.,1.71022579061586E-31));
#26427=DIRECTION('ref_axis',(0.338210048707227,2.25179828655966E-17,0.941070647163886));
#26428=DIRECTION('',(6.65798752924967E-17,-1.,1.71022579061586E-31));
#26429=DIRECTION('center_axis',(6.65798752924967E-17,-1.,1.71022579061586E-31));
#26430=DIRECTION('ref_axis',(0.338210048713215,2.25179828659953E-17,0.941070647161734));
#26431=DIRECTION('',(-6.65798752924967E-17,1.,-1.71022579061586E-31));
#26432=DIRECTION('center_axis',(-6.65798752924967E-17,1.,-1.71022579061586E-31));
#26433=DIRECTION('ref_axis',(0.338210048713215,2.25179828659953E-17,0.941070647161734));
#26434=DIRECTION('center_axis',(6.65798752924967E-17,-1.,1.71022579061586E-31));
#26435=DIRECTION('ref_axis',(0.203946891574005,1.35787586072898E-17,0.978981953570801));
#26436=DIRECTION('',(6.65798752924967E-17,-1.,1.71022579061586E-31));
#26437=DIRECTION('center_axis',(6.65798752924967E-17,-1.,1.71022579061586E-31));
#26438=DIRECTION('ref_axis',(0.203946891583929,1.35787586079505E-17,0.978981953568733));
#26439=DIRECTION('',(-6.65798752924967E-17,1.,-1.71022579061586E-31));
#26440=DIRECTION('center_axis',(-6.65798752924967E-17,1.,-1.71022579061586E-31));
#26441=DIRECTION('ref_axis',(0.203946891583929,1.35787586079505E-17,0.978981953568733));
#26442=DIRECTION('center_axis',(6.65798752924967E-17,-1.,1.71022579061586E-31));
#26443=DIRECTION('ref_axis',(0.0657141401824452,4.37523925830102E-18,0.997838489826927));
#26444=DIRECTION('',(6.65798752924967E-17,-1.,1.71022579061586E-31));
#26445=DIRECTION('center_axis',(6.65798752924967E-17,-1.,1.71022579061586E-31));
#26446=DIRECTION('ref_axis',(0.0657141401961282,4.37523925921203E-18,0.997838489826026));
#26447=DIRECTION('',(-6.65798752924967E-17,1.,-1.71022579061586E-31));
#26448=DIRECTION('center_axis',(-6.65798752924967E-17,1.,-1.71022579061586E-31));
#26449=DIRECTION('ref_axis',(0.0657141401961282,4.37523925921203E-18,0.997838489826026));
#26450=DIRECTION('center_axis',(6.65798752924967E-17,-1.,1.71022579061586E-31));
#26451=DIRECTION('ref_axis',(-0.0737976621990395,-4.91343914608968E-18,
0.997273234903031));
#26452=DIRECTION('',(6.65798752924967E-17,-1.,1.71022579061586E-31));
#26453=DIRECTION('center_axis',(6.65798752924967E-17,-1.,1.71022579061586E-31));
#26454=DIRECTION('ref_axis',(-0.073797662182064,-4.91343914495945E-18,0.997273234904287));
#26455=DIRECTION('',(-6.65798752924967E-17,1.,-1.71022579061586E-31));
#26456=DIRECTION('center_axis',(-6.65798752924967E-17,1.,-1.71022579061586E-31));
#26457=DIRECTION('ref_axis',(-0.073797662182064,-4.91343914495945E-18,0.997273234904287));
#26458=DIRECTION('center_axis',(-6.65798752924967E-17,1.,-1.71022579061586E-31));
#26459=DIRECTION('ref_axis',(-0.211873077029416,-1.41064830464559E-17,0.97729719084324));
#26460=DIRECTION('center_axis',(-6.65798752924967E-17,1.,-1.71022579061586E-31));
#26461=DIRECTION('ref_axis',(-0.211873077029416,-1.41064830464559E-17,0.97729719084324));
#26462=DIRECTION('center_axis',(6.65798752924967E-17,-1.,1.71022579061586E-31));
#26463=DIRECTION('ref_axis',(-0.211873077029416,-1.41064830464559E-17,0.977297190843239));
#26464=DIRECTION('center_axis',(-6.65798752924967E-17,1.,-1.71022579061586E-31));
#26465=DIRECTION('ref_axis',(-0.211873077029416,-1.41064830464559E-17,0.97729719084324));
#26466=DIRECTION('center_axis',(-6.65798752924967E-17,1.,-1.71022579061586E-31));
#26467=DIRECTION('ref_axis',(-0.211873077029416,-1.41064830464559E-17,0.97729719084324));
#26468=DIRECTION('center_axis',(-6.65798752924967E-17,1.,-1.71022579061586E-31));
#26469=DIRECTION('ref_axis',(-0.211873077029416,-1.41064830464559E-17,0.97729719084324));
#26470=DIRECTION('center_axis',(-6.65798752924967E-17,1.,-1.71022579061586E-31));
#26471=DIRECTION('ref_axis',(-0.211873077029416,-1.41064830464559E-17,0.97729719084324));
#26472=DIRECTION('center_axis',(-6.65798752924967E-17,1.,-1.71022579061586E-31));
#26473=DIRECTION('ref_axis',(-0.211873077029416,-1.41064830464559E-17,0.97729719084324));
#26474=DIRECTION('center_axis',(-6.65798752924967E-17,1.,-1.71022579061586E-31));
#26475=DIRECTION('ref_axis',(-0.211873077029416,-1.41064830464559E-17,0.97729719084324));
#26476=DIRECTION('center_axis',(-6.65798752924967E-17,1.,-1.71022579061586E-31));
#26477=DIRECTION('ref_axis',(-0.211873077029416,-1.41064830464559E-17,0.97729719084324));
#26478=DIRECTION('center_axis',(-6.65798752924967E-17,1.,-1.71022579061586E-31));
#26479=DIRECTION('ref_axis',(-0.211873077029416,-1.41064830464559E-17,0.97729719084324));
#26480=DIRECTION('center_axis',(-6.65798752924967E-17,1.,-1.71022579061586E-31));
#26481=DIRECTION('ref_axis',(-0.211873077029416,-1.41064830464559E-17,0.97729719084324));
#26482=DIRECTION('center_axis',(-6.65798752924967E-17,1.,-1.71022579061586E-31));
#26483=DIRECTION('ref_axis',(-0.211873077029416,-1.41064830464559E-17,0.97729719084324));
#26484=DIRECTION('center_axis',(-6.65798752924967E-17,1.,-1.71022579061586E-31));
#26485=DIRECTION('ref_axis',(-0.211873077029416,-1.41064830464559E-17,0.97729719084324));
#26486=DIRECTION('center_axis',(-6.65798752924967E-17,1.,-1.71022579061586E-31));
#26487=DIRECTION('ref_axis',(-0.211873077029416,-1.41064830464559E-17,0.97729719084324));
#26488=DIRECTION('center_axis',(-6.65798752924967E-17,1.,-1.71022579061586E-31));
#26489=DIRECTION('ref_axis',(-0.211873077029416,-1.41064830464559E-17,0.97729719084324));
#26490=DIRECTION('center_axis',(-6.65798752924967E-17,1.,-1.71022579061586E-31));
#26491=DIRECTION('ref_axis',(-0.211873077029416,-1.41064830464559E-17,0.97729719084324));
#26492=DIRECTION('center_axis',(-6.65798752924967E-17,1.,-1.71022579061586E-31));
#26493=DIRECTION('ref_axis',(-0.211873077029416,-1.41064830464559E-17,0.97729719084324));
#26494=DIRECTION('center_axis',(-6.65798752924967E-17,1.,-1.71022579061586E-31));
#26495=DIRECTION('ref_axis',(-0.211873077029416,-1.41064830464559E-17,0.97729719084324));
#26496=DIRECTION('center_axis',(-6.65798752924967E-17,1.,-1.71022579061586E-31));
#26497=DIRECTION('ref_axis',(-0.211873077029416,-1.41064830464559E-17,0.97729719084324));
#26498=DIRECTION('center_axis',(-6.65798752924967E-17,1.,-1.71022579061586E-31));
#26499=DIRECTION('ref_axis',(-0.211873077029416,-1.41064830464559E-17,0.97729719084324));
#26500=DIRECTION('center_axis',(-6.65798752924967E-17,1.,-1.71022579061586E-31));
#26501=DIRECTION('ref_axis',(-0.211873077029416,-1.41064830464559E-17,0.97729719084324));
#26502=DIRECTION('center_axis',(-6.65798752924967E-17,1.,-1.71022579061586E-31));
#26503=DIRECTION('ref_axis',(-0.211873077029416,-1.41064830464559E-17,0.97729719084324));
#26504=DIRECTION('center_axis',(-6.65798752924967E-17,1.,-1.71022579061586E-31));
#26505=DIRECTION('ref_axis',(-0.211873077029416,-1.41064830464559E-17,0.97729719084324));
#26506=DIRECTION('center_axis',(-6.65798752924967E-17,1.,-1.71022579061586E-31));
#26507=DIRECTION('ref_axis',(-0.211873077029416,-1.41064830464559E-17,0.97729719084324));
#26508=DIRECTION('center_axis',(-6.65798752924967E-17,1.,-1.71022579061586E-31));
#26509=DIRECTION('ref_axis',(-0.211873077029416,-1.41064830464559E-17,0.97729719084324));
#26510=DIRECTION('center_axis',(-6.65798752924967E-17,1.,-1.71022579061586E-31));
#26511=DIRECTION('ref_axis',(-0.211873077029416,-1.41064830464559E-17,0.97729719084324));
#26512=DIRECTION('center_axis',(-6.65798752924967E-17,1.,-1.71022579061586E-31));
#26513=DIRECTION('ref_axis',(-0.211873077029416,-1.41064830464559E-17,0.97729719084324));
#26514=DIRECTION('center_axis',(-6.65798752924967E-17,1.,-1.71022579061586E-31));
#26515=DIRECTION('ref_axis',(-0.211873077029416,-1.41064830464559E-17,0.97729719084324));
#26516=DIRECTION('center_axis',(-6.65798752924967E-17,1.,-1.71022579061586E-31));
#26517=DIRECTION('ref_axis',(-0.211873077029416,-1.41064830464559E-17,0.97729719084324));
#26518=DIRECTION('center_axis',(-6.65798752924967E-17,1.,-1.71022579061586E-31));
#26519=DIRECTION('ref_axis',(-0.211873077029416,-1.41064830464559E-17,0.97729719084324));
#26520=DIRECTION('center_axis',(-6.65798752924967E-17,1.,-1.71022579061586E-31));
#26521=DIRECTION('ref_axis',(-0.211873077029416,-1.41064830464559E-17,0.97729719084324));
#26522=DIRECTION('center_axis',(-6.65798752924967E-17,1.,-1.71022579061586E-31));
#26523=DIRECTION('ref_axis',(-0.211873077029416,-1.41064830464559E-17,0.97729719084324));
#26524=DIRECTION('center_axis',(-6.65798752924967E-17,1.,-1.71022579061586E-31));
#26525=DIRECTION('ref_axis',(-0.211873077029416,-1.41064830464559E-17,0.97729719084324));
#26526=DIRECTION('center_axis',(-6.65798752924967E-17,1.,-1.71022579061586E-31));
#26527=DIRECTION('ref_axis',(-0.211873077029416,-1.41064830464559E-17,0.97729719084324));
#26528=DIRECTION('center_axis',(-6.65798752924967E-17,1.,-1.71022579061586E-31));
#26529=DIRECTION('ref_axis',(-0.211873077029416,-1.41064830464559E-17,0.97729719084324));
#26530=DIRECTION('center_axis',(-6.65798752924967E-17,1.,-1.71022579061586E-31));
#26531=DIRECTION('ref_axis',(-0.211873077029416,-1.41064830464559E-17,0.97729719084324));
#26532=DIRECTION('center_axis',(-6.65798752924967E-17,1.,-1.71022579061586E-31));
#26533=DIRECTION('ref_axis',(-0.211873077029416,-1.41064830464559E-17,0.97729719084324));
#26534=DIRECTION('center_axis',(-6.65798752924967E-17,1.,-1.71022579061586E-31));
#26535=DIRECTION('ref_axis',(-0.211873077029416,-1.41064830464559E-17,0.97729719084324));
#26536=DIRECTION('center_axis',(-6.65798752924967E-17,1.,-1.71022579061586E-31));
#26537=DIRECTION('ref_axis',(-0.211873077029416,-1.41064830464559E-17,0.97729719084324));
#26538=DIRECTION('center_axis',(-6.65798752924967E-17,1.,-1.71022579061586E-31));
#26539=DIRECTION('ref_axis',(-0.211873077029416,-1.41064830464559E-17,0.97729719084324));
#26540=DIRECTION('center_axis',(-6.65798752924967E-17,1.,-1.71022579061586E-31));
#26541=DIRECTION('ref_axis',(-0.211873077029416,-1.41064830464559E-17,0.97729719084324));
#26542=DIRECTION('center_axis',(-6.65798752924967E-17,1.,-1.71022579061586E-31));
#26543=DIRECTION('ref_axis',(-0.211873077029416,-1.41064830464559E-17,0.97729719084324));
#26544=DIRECTION('center_axis',(-6.65798752924967E-17,1.,-1.71022579061586E-31));
#26545=DIRECTION('ref_axis',(-0.211873077029416,-1.41064830464559E-17,0.97729719084324));
#26546=DIRECTION('center_axis',(-6.65798752924967E-17,1.,-1.71022579061586E-31));
#26547=DIRECTION('ref_axis',(-0.211873077029416,-1.41064830464559E-17,0.97729719084324));
#26548=DIRECTION('center_axis',(-6.65798752924967E-17,1.,-1.71022579061586E-31));
#26549=DIRECTION('ref_axis',(-0.211873077029416,-1.41064830464559E-17,0.97729719084324));
#26550=DIRECTION('center_axis',(-6.65798752924967E-17,1.,-1.71022579061586E-31));
#26551=DIRECTION('ref_axis',(-0.211873077029416,-1.41064830464559E-17,0.97729719084324));
#26552=DIRECTION('center_axis',(6.65798752924967E-17,-1.,1.71022579061586E-31));
#26553=DIRECTION('ref_axis',(0.211873077029416,1.41064830464559E-17,-0.977297190843239));
#26554=DIRECTION('center_axis',(-6.65798752924967E-17,1.,-1.71022579061586E-31));
#26555=DIRECTION('ref_axis',(-0.211873077029416,-1.41064830464559E-17,0.977297190843239));
#26556=DIRECTION('center_axis',(-6.65798752924967E-17,1.,-1.71022579061586E-31));
#26557=DIRECTION('ref_axis',(-0.211873077029416,-1.41064830464559E-17,0.97729719084324));
#26558=DIRECTION('',(-6.65798752924967E-17,1.,-1.71022579061586E-31));
#26559=DIRECTION('center_axis',(-6.65798752924967E-17,1.,-1.71022579061586E-31));
#26560=DIRECTION('ref_axis',(-0.211873077029416,-1.41064830464559E-17,0.977297190843239));
#26561=DIRECTION('',(6.65798752924967E-17,-1.,1.71022579061586E-31));
#26562=DIRECTION('center_axis',(-6.65798752924967E-17,1.,-1.71022579061586E-31));
#26563=DIRECTION('ref_axis',(-0.211873077029416,-1.41064830464559E-17,0.97729719084324));
#26564=DIRECTION('center_axis',(-6.65798752924967E-17,1.,-1.71022579061586E-31));
#26565=DIRECTION('ref_axis',(-0.211873077029416,-1.41064830464559E-17,0.977297190843239));
#26566=DIRECTION('center_axis',(-6.65798752924967E-17,1.,-1.71022579061586E-31));
#26567=DIRECTION('ref_axis',(-0.211873077029416,-1.41064830464559E-17,0.97729719084324));
#26568=DIRECTION('center_axis',(-6.65798752924967E-17,1.,-1.71022579061586E-31));
#26569=DIRECTION('ref_axis',(-0.211873077029416,-1.41064830464559E-17,0.977297190843239));
#26570=DIRECTION('center_axis',(-6.65798752924967E-17,1.,-1.71022579061586E-31));
#26571=DIRECTION('ref_axis',(-0.211873077029416,-1.41064830464559E-17,0.97729719084324));
#26572=DIRECTION('center_axis',(-6.65798752924967E-17,1.,-1.71022579061586E-31));
#26573=DIRECTION('ref_axis',(-0.211873077029416,-1.41064830464559E-17,0.977297190843239));
#26574=DIRECTION('center_axis',(-6.65798752924967E-17,1.,-1.71022579061586E-31));
#26575=DIRECTION('ref_axis',(-0.211873077029416,-1.41064830464559E-17,0.97729719084324));
#26576=DIRECTION('center_axis',(-6.65798752924967E-17,1.,-1.71022579061586E-31));
#26577=DIRECTION('ref_axis',(-0.211873077029416,-1.41064830464559E-17,0.977297190843239));
#26578=DIRECTION('center_axis',(-6.65798752924967E-17,1.,-1.71022579061586E-31));
#26579=DIRECTION('ref_axis',(-0.211873077029416,-1.41064830464559E-17,0.97729719084324));
#26580=DIRECTION('center_axis',(-6.65798752924967E-17,1.,-1.71022579061586E-31));
#26581=DIRECTION('ref_axis',(-0.211873077029416,-1.41064830464559E-17,0.977297190843239));
#26582=DIRECTION('center_axis',(-6.65798752924967E-17,1.,-1.71022579061586E-31));
#26583=DIRECTION('ref_axis',(-0.211873077029416,-1.41064830464559E-17,0.97729719084324));
#26584=DIRECTION('center_axis',(-6.65798752924967E-17,1.,-1.71022579061586E-31));
#26585=DIRECTION('ref_axis',(-0.211873077029416,-1.41064830464559E-17,0.977297190843239));
#26586=DIRECTION('center_axis',(-6.65798752924967E-17,1.,-1.71022579061586E-31));
#26587=DIRECTION('ref_axis',(-0.211873077029416,-1.41064830464559E-17,0.97729719084324));
#26588=DIRECTION('center_axis',(-6.65798752924967E-17,1.,-1.71022579061586E-31));
#26589=DIRECTION('ref_axis',(-0.211873077029416,-1.41064830464559E-17,0.977297190843239));
#26590=DIRECTION('center_axis',(-6.65798752924967E-17,1.,-1.71022579061586E-31));
#26591=DIRECTION('ref_axis',(-0.211873077029416,-1.41064830464559E-17,0.97729719084324));
#26592=DIRECTION('center_axis',(-6.65798752924967E-17,1.,-1.71022579061586E-31));
#26593=DIRECTION('ref_axis',(-0.211873077029416,-1.41064830464559E-17,0.977297190843239));
#26594=DIRECTION('center_axis',(-6.65798752924967E-17,1.,-1.71022579061586E-31));
#26595=DIRECTION('ref_axis',(-0.211873077029416,-1.41064830464559E-17,0.97729719084324));
#26596=DIRECTION('center_axis',(-6.65798752924967E-17,1.,-1.71022579061586E-31));
#26597=DIRECTION('ref_axis',(-0.211873077029416,-1.41064830464559E-17,0.977297190843239));
#26598=DIRECTION('center_axis',(-6.65798752924967E-17,1.,-1.71022579061586E-31));
#26599=DIRECTION('ref_axis',(-0.211873077029416,-1.41064830464559E-17,0.97729719084324));
#26600=DIRECTION('center_axis',(-6.65798752924967E-17,1.,-1.71022579061586E-31));
#26601=DIRECTION('ref_axis',(-0.211873077029416,-1.41064830464559E-17,0.977297190843239));
#26602=DIRECTION('center_axis',(-6.65798752924967E-17,1.,-1.71022579061586E-31));
#26603=DIRECTION('ref_axis',(-0.211873077029416,-1.41064830464559E-17,0.97729719084324));
#26604=DIRECTION('center_axis',(-6.65798752924967E-17,1.,-1.71022579061586E-31));
#26605=DIRECTION('ref_axis',(-0.211873077029416,-1.41064830464559E-17,0.977297190843239));
#26606=DIRECTION('center_axis',(-6.65798752924967E-17,1.,-1.71022579061586E-31));
#26607=DIRECTION('ref_axis',(-0.211873077029416,-1.41064830464559E-17,0.97729719084324));
#26608=DIRECTION('center_axis',(-6.65798752924967E-17,1.,-1.71022579061586E-31));
#26609=DIRECTION('ref_axis',(-0.211873077029416,-1.41064830464559E-17,0.977297190843239));
#26610=DIRECTION('center_axis',(-6.65798752924967E-17,1.,-1.71022579061586E-31));
#26611=DIRECTION('ref_axis',(-0.211873077029416,-1.41064830464559E-17,0.97729719084324));
#26612=DIRECTION('center_axis',(-6.65798752924967E-17,1.,-1.71022579061586E-31));
#26613=DIRECTION('ref_axis',(-0.211873077029416,-1.41064830464559E-17,0.977297190843239));
#26614=DIRECTION('center_axis',(-6.65798752924967E-17,1.,-1.71022579061586E-31));
#26615=DIRECTION('ref_axis',(-0.211873077029416,-1.41064830464559E-17,0.97729719084324));
#26616=DIRECTION('center_axis',(-6.65798752924967E-17,1.,-1.71022579061586E-31));
#26617=DIRECTION('ref_axis',(-0.211873077029416,-1.41064830464559E-17,0.977297190843239));
#26618=DIRECTION('center_axis',(-6.65798752924967E-17,1.,-1.71022579061586E-31));
#26619=DIRECTION('ref_axis',(-0.211873077029416,-1.41064830464559E-17,0.97729719084324));
#26620=DIRECTION('center_axis',(-6.65798752924967E-17,1.,-1.71022579061586E-31));
#26621=DIRECTION('ref_axis',(-0.211873077029416,-1.41064830464559E-17,0.977297190843239));
#26622=DIRECTION('center_axis',(-6.65798752924967E-17,1.,-1.71022579061586E-31));
#26623=DIRECTION('ref_axis',(-0.211873077029416,-1.41064830464559E-17,0.97729719084324));
#26624=DIRECTION('center_axis',(-6.65798752924967E-17,1.,-1.71022579061586E-31));
#26625=DIRECTION('ref_axis',(-0.211873077029416,-1.41064830464559E-17,0.977297190843239));
#26626=DIRECTION('center_axis',(-6.65798752924967E-17,1.,-1.71022579061586E-31));
#26627=DIRECTION('ref_axis',(-0.211873077029416,-1.41064830464559E-17,0.97729719084324));
#26628=DIRECTION('center_axis',(-6.65798752924967E-17,1.,-1.71022579061586E-31));
#26629=DIRECTION('ref_axis',(-0.211873077029416,-1.41064830464559E-17,0.977297190843239));
#26630=DIRECTION('center_axis',(-6.65798752924967E-17,1.,-1.71022579061586E-31));
#26631=DIRECTION('ref_axis',(-0.211873077029416,-1.41064830464559E-17,0.97729719084324));
#26632=DIRECTION('center_axis',(-6.65798752924967E-17,1.,-1.71022579061586E-31));
#26633=DIRECTION('ref_axis',(-0.211873077029416,-1.41064830464559E-17,0.977297190843239));
#26634=DIRECTION('center_axis',(-6.65798752924967E-17,1.,-1.71022579061586E-31));
#26635=DIRECTION('ref_axis',(-0.211873077029416,-1.41064830464559E-17,0.97729719084324));
#26636=DIRECTION('center_axis',(-6.65798752924967E-17,1.,-1.71022579061586E-31));
#26637=DIRECTION('ref_axis',(-0.211873077029416,-1.41064830464559E-17,0.977297190843239));
#26638=DIRECTION('center_axis',(-6.65798752924967E-17,1.,-1.71022579061586E-31));
#26639=DIRECTION('ref_axis',(-0.211873077029416,-1.41064830464559E-17,0.97729719084324));
#26640=DIRECTION('center_axis',(-6.65798752924967E-17,1.,-1.71022579061586E-31));
#26641=DIRECTION('ref_axis',(-0.211873077029416,-1.41064830464559E-17,0.977297190843239));
#26642=DIRECTION('center_axis',(-6.65798752924967E-17,1.,-1.71022579061586E-31));
#26643=DIRECTION('ref_axis',(-0.211873077029416,-1.41064830464559E-17,0.97729719084324));
#26644=DIRECTION('center_axis',(-6.65798752924967E-17,1.,-1.71022579061586E-31));
#26645=DIRECTION('ref_axis',(-0.211873077029416,-1.41064830464559E-17,0.977297190843239));
#26646=DIRECTION('center_axis',(-6.65798752924967E-17,1.,-1.71022579061586E-31));
#26647=DIRECTION('ref_axis',(-0.211873077029416,-1.41064830464559E-17,0.97729719084324));
#26648=DIRECTION('center_axis',(-6.65798752924967E-17,1.,-1.71022579061586E-31));
#26649=DIRECTION('ref_axis',(-0.211873077029416,-1.41064830464559E-17,0.977297190843239));
#26650=DIRECTION('center_axis',(-6.65798752924967E-17,1.,-1.71022579061586E-31));
#26651=DIRECTION('ref_axis',(-0.211873077029416,-1.41064830464559E-17,0.97729719084324));
#26652=DIRECTION('center_axis',(-6.65798752924967E-17,1.,-1.71022579061586E-31));
#26653=DIRECTION('ref_axis',(-0.211873077029416,-1.41064830464559E-17,0.977297190843239));
#26654=DIRECTION('center_axis',(-6.65798752924967E-17,1.,-1.71022579061586E-31));
#26655=DIRECTION('ref_axis',(-0.211873077029416,-1.41064830464559E-17,0.97729719084324));
#26656=DIRECTION('center_axis',(-6.65798752924967E-17,1.,-1.71022579061586E-31));
#26657=DIRECTION('ref_axis',(-0.211873077029416,-1.41064830464559E-17,0.977297190843239));
#26658=DIRECTION('center_axis',(-6.65798752924967E-17,1.,-1.71022579061586E-31));
#26659=DIRECTION('ref_axis',(-0.211873077029416,-1.41064830464559E-17,0.97729719084324));
#26660=DIRECTION('center_axis',(-6.65798752924967E-17,1.,-1.71022579061586E-31));
#26661=DIRECTION('ref_axis',(-0.211873077029416,-1.41064830464559E-17,0.977297190843239));
#26662=DIRECTION('center_axis',(-6.65798752924967E-17,1.,-1.71022579061586E-31));
#26663=DIRECTION('ref_axis',(-0.211873077029416,-1.41064830464559E-17,0.97729719084324));
#26664=DIRECTION('center_axis',(-6.65798752924967E-17,1.,-1.71022579061586E-31));
#26665=DIRECTION('ref_axis',(-0.211873077029416,-1.41064830464559E-17,0.977297190843239));
#26666=DIRECTION('center_axis',(-6.65798752924967E-17,1.,-1.71022579061586E-31));
#26667=DIRECTION('ref_axis',(-0.211873077029416,-1.41064830464559E-17,0.97729719084324));
#26668=DIRECTION('center_axis',(-6.65798752924967E-17,1.,-1.71022579061586E-31));
#26669=DIRECTION('ref_axis',(-0.211873077029416,-1.41064830464559E-17,0.977297190843239));
#26670=DIRECTION('center_axis',(-6.65798752924967E-17,1.,-1.71022579061586E-31));
#26671=DIRECTION('ref_axis',(-0.211873077029416,-1.41064830464559E-17,0.97729719084324));
#26672=DIRECTION('center_axis',(-6.65798752924967E-17,1.,-1.71022579061586E-31));
#26673=DIRECTION('ref_axis',(-0.211873077029416,-1.41064830464559E-17,0.977297190843239));
#26674=DIRECTION('center_axis',(-6.65798752924967E-17,1.,-1.71022579061586E-31));
#26675=DIRECTION('ref_axis',(-0.211873077029416,-1.41064830464559E-17,0.97729719084324));
#26676=DIRECTION('center_axis',(-6.65798752924967E-17,1.,-1.71022579061586E-31));
#26677=DIRECTION('ref_axis',(-0.211873077029416,-1.41064830464559E-17,0.977297190843239));
#26678=DIRECTION('center_axis',(-6.65798752924967E-17,1.,-1.71022579061586E-31));
#26679=DIRECTION('ref_axis',(-0.211873077029416,-1.41064830464559E-17,0.97729719084324));
#26680=DIRECTION('center_axis',(-6.65798752924967E-17,1.,-1.71022579061586E-31));
#26681=DIRECTION('ref_axis',(-0.211873077029416,-1.41064830464559E-17,0.977297190843239));
#26682=DIRECTION('center_axis',(-6.65798752924967E-17,1.,-1.71022579061586E-31));
#26683=DIRECTION('ref_axis',(-0.211873077029416,-1.41064830464559E-17,0.97729719084324));
#26684=DIRECTION('center_axis',(-6.65798752924967E-17,1.,-1.71022579061586E-31));
#26685=DIRECTION('ref_axis',(-0.211873077029416,-1.41064830464559E-17,0.977297190843239));
#26686=DIRECTION('center_axis',(-6.65798752924967E-17,1.,-1.71022579061586E-31));
#26687=DIRECTION('ref_axis',(-0.211873077029416,-1.41064830464559E-17,0.97729719084324));
#26688=DIRECTION('center_axis',(-6.65798752924967E-17,1.,-1.71022579061586E-31));
#26689=DIRECTION('ref_axis',(-0.211873077029416,-1.41064830464559E-17,0.977297190843239));
#26690=DIRECTION('center_axis',(-6.65798752924967E-17,1.,-1.71022579061586E-31));
#26691=DIRECTION('ref_axis',(-0.211873077029416,-1.41064830464559E-17,0.97729719084324));
#26692=DIRECTION('center_axis',(-6.65798752924967E-17,1.,-1.71022579061586E-31));
#26693=DIRECTION('ref_axis',(-0.211873077029416,-1.41064830464559E-17,0.977297190843239));
#26694=DIRECTION('center_axis',(-6.65798752924967E-17,1.,-1.71022579061586E-31));
#26695=DIRECTION('ref_axis',(-0.211873077029416,-1.41064830464559E-17,0.97729719084324));
#26696=DIRECTION('center_axis',(-6.65798752924967E-17,1.,-1.71022579061586E-31));
#26697=DIRECTION('ref_axis',(-0.211873077029416,-1.41064830464559E-17,0.977297190843239));
#26698=DIRECTION('center_axis',(-6.65798752924967E-17,1.,-1.71022579061586E-31));
#26699=DIRECTION('ref_axis',(-0.211873077029416,-1.41064830464559E-17,0.97729719084324));
#26700=DIRECTION('center_axis',(-6.65798752924967E-17,1.,-1.71022579061586E-31));
#26701=DIRECTION('ref_axis',(-0.211873077029416,-1.41064830464559E-17,0.977297190843239));
#26702=DIRECTION('center_axis',(-6.65798752924967E-17,1.,-1.71022579061586E-31));
#26703=DIRECTION('ref_axis',(-0.211873077029416,-1.41064830464559E-17,0.97729719084324));
#26704=DIRECTION('center_axis',(-6.65798752924967E-17,1.,-1.71022579061586E-31));
#26705=DIRECTION('ref_axis',(-0.211873077029416,-1.41064830464559E-17,0.977297190843239));
#26706=DIRECTION('center_axis',(-6.65798752924967E-17,1.,-1.71022579061586E-31));
#26707=DIRECTION('ref_axis',(-0.211873077029416,-1.41064830464559E-17,0.97729719084324));
#26708=DIRECTION('center_axis',(-6.65798752924967E-17,1.,-1.71022579061586E-31));
#26709=DIRECTION('ref_axis',(-0.211873077029416,-1.41064830464559E-17,0.977297190843239));
#26710=DIRECTION('center_axis',(-6.65798752924967E-17,1.,-1.71022579061586E-31));
#26711=DIRECTION('ref_axis',(-0.211873077029416,-1.41064830464559E-17,0.97729719084324));
#26712=DIRECTION('center_axis',(-6.65798752924967E-17,1.,-1.71022579061586E-31));
#26713=DIRECTION('ref_axis',(-0.211873077029416,-1.41064830464559E-17,0.977297190843239));
#26714=DIRECTION('center_axis',(-6.65798752924967E-17,1.,-1.71022579061586E-31));
#26715=DIRECTION('ref_axis',(-0.211873077029416,-1.41064830464559E-17,0.97729719084324));
#26716=DIRECTION('center_axis',(-6.65798752924967E-17,1.,-1.71022579061586E-31));
#26717=DIRECTION('ref_axis',(-0.211873077029416,-1.41064830464559E-17,0.977297190843239));
#26718=DIRECTION('center_axis',(-6.65798752924967E-17,1.,-1.71022579061586E-31));
#26719=DIRECTION('ref_axis',(-0.211873077029416,-1.41064830464559E-17,0.97729719084324));
#26720=DIRECTION('center_axis',(-6.65798752924967E-17,1.,-1.71022579061586E-31));
#26721=DIRECTION('ref_axis',(-0.211873077029416,-1.41064830464559E-17,0.977297190843239));
#26722=DIRECTION('center_axis',(-6.65798752924967E-17,1.,-1.71022579061586E-31));
#26723=DIRECTION('ref_axis',(-0.211873077029416,-1.41064830464559E-17,0.97729719084324));
#26724=DIRECTION('center_axis',(-6.65798752924967E-17,1.,-1.71022579061586E-31));
#26725=DIRECTION('ref_axis',(-0.211873077029416,-1.41064830464559E-17,0.977297190843239));
#26726=DIRECTION('center_axis',(-6.65798752924967E-17,1.,-1.71022579061586E-31));
#26727=DIRECTION('ref_axis',(-0.211873077029416,-1.41064830464559E-17,0.97729719084324));
#26728=DIRECTION('center_axis',(-6.65798752924967E-17,1.,-1.71022579061586E-31));
#26729=DIRECTION('ref_axis',(-0.211873077029416,-1.41064830464559E-17,0.977297190843239));
#26730=DIRECTION('center_axis',(-6.65798752924967E-17,1.,-1.71022579061586E-31));
#26731=DIRECTION('ref_axis',(-0.211873077029416,-1.41064830464559E-17,0.97729719084324));
#26732=DIRECTION('center_axis',(6.65798752924967E-17,-1.,1.71022579061586E-31));
#26733=DIRECTION('ref_axis',(-0.211873077029416,-1.41064830464559E-17,0.977297190843239));
#26734=DIRECTION('center_axis',(-6.65798752924967E-17,1.,-1.71022579061586E-31));
#26735=DIRECTION('ref_axis',(-0.211873077029416,-1.41064830464559E-17,0.977297190843239));
#26736=DIRECTION('center_axis',(-6.65798752924967E-17,1.,-1.71022579061586E-31));
#26737=DIRECTION('ref_axis',(-0.211873077029416,-1.41064830464559E-17,0.97729719084324));
#26738=DIRECTION('center_axis',(-6.65798752924967E-17,1.,-1.71022579061586E-31));
#26739=DIRECTION('ref_axis',(-0.211873077029416,-1.41064830464559E-17,0.97729719084324));
#26740=DIRECTION('center_axis',(6.65798752924967E-17,-1.,1.71022579061586E-31));
#26741=DIRECTION('ref_axis',(0.211873077029416,1.41064830464559E-17,-0.977297190843239));
#26742=DIRECTION('center_axis',(-6.65798752924967E-17,1.,-1.71022579061586E-31));
#26743=DIRECTION('ref_axis',(-0.211873077029416,-1.41064830464559E-17,0.977297190843239));
#26744=DIRECTION('center_axis',(-6.65798752924967E-17,1.,-1.71022579061586E-31));
#26745=DIRECTION('ref_axis',(0.211873077029416,1.41064830464559E-17,-0.97729719084324));
#26746=DIRECTION('',(-6.65798752924967E-17,1.,-1.71022579061586E-31));
#26747=DIRECTION('axis',(0.,0.,1.));
#26748=DIRECTION('refdir',(1.,0.,0.));
#26749=DIRECTION('center_axis',(6.12323404134149E-17,-1.,3.14444500472474E-32));
#26750=DIRECTION('ref_axis',(1.55749764652046E-5,0.,-0.99999999987871));
#26751=DIRECTION('center_axis',(-6.12323404134149E-17,1.,-3.14444500472474E-32));
#26752=DIRECTION('ref_axis',(-0.99999999987871,-6.1232340405988E-17,-1.55749724650822E-5));
#26753=DIRECTION('center_axis',(-0.99999999987871,-6.1232340405988E-17,
-1.55749764653271E-5));
#26754=DIRECTION('ref_axis',(-1.55749764653271E-5,0.,0.99999999987871));
#26755=DIRECTION('center_axis',(6.12323404134149E-17,-1.,3.14444500472474E-32));
#26756=DIRECTION('ref_axis',(-0.99999999987871,-6.1232340405988E-17,-1.55749728614786E-5));
#26757=DIRECTION('center_axis',(-6.12323404134149E-17,1.,-3.14444500472474E-32));
#26758=DIRECTION('ref_axis',(-0.99999999987871,-6.1232340405988E-17,-1.55749724650822E-5));
#26759=DIRECTION('center_axis',(6.12323404134149E-17,-1.,3.14444500472474E-32));
#26760=DIRECTION('ref_axis',(0.99999999987871,6.1232340405988E-17,1.55749764652046E-5));
#26761=DIRECTION('center_axis',(6.12323404134149E-17,-1.,3.14444500472474E-32));
#26762=DIRECTION('ref_axis',(-0.99999999987871,-6.1232340405988E-17,-1.55749724650822E-5));
#26763=DIRECTION('',(6.12323404134149E-17,-1.,3.14444500472474E-32));
#26764=DIRECTION('center_axis',(6.12323404134149E-17,-1.,3.14444500472474E-32));
#26765=DIRECTION('ref_axis',(-0.99999999987871,-6.1232340405988E-17,-1.55749724650822E-5));
#26766=DIRECTION('center_axis',(6.12323404134149E-17,-1.,3.14444500472474E-32));
#26767=DIRECTION('ref_axis',(0.99999999987871,6.12323404059881E-17,1.55749764652046E-5));
#26768=DIRECTION('center_axis',(6.12323404134149E-17,-1.,3.14444500472474E-32));
#26769=DIRECTION('ref_axis',(0.99999999987871,6.1232340405988E-17,1.55749764652046E-5));
#26770=DIRECTION('center_axis',(6.12323404134149E-17,-1.,3.14444500472474E-32));
#26771=DIRECTION('ref_axis',(1.55749764652046E-5,0.,-0.99999999987871));
#26772=DIRECTION('center_axis',(-6.12323404134149E-17,1.,-3.14444500472474E-32));
#26773=DIRECTION('ref_axis',(-0.99999999987871,-6.1232340405988E-17,-1.55749728614786E-5));
#26774=DIRECTION('center_axis',(-0.99999999987871,-6.1232340405988E-17,
-1.55749764653271E-5));
#26775=DIRECTION('ref_axis',(-1.55749764653271E-5,0.,0.99999999987871));
#26776=DIRECTION('center_axis',(-6.12323404134149E-17,1.,-3.14444500472474E-32));
#26777=DIRECTION('ref_axis',(-1.55749764652046E-5,-9.53692260816889E-22,
0.99999999987871));
#26778=DIRECTION('center_axis',(6.12323404134149E-17,-1.,3.14444500472474E-32));
#26779=DIRECTION('ref_axis',(0.99999999987871,6.1232340405988E-17,1.55749764652046E-5));
#26780=DIRECTION('center_axis',(6.12323404134149E-17,-1.,3.14444500472474E-32));
#26781=DIRECTION('ref_axis',(0.99999999987871,6.1232340405988E-17,1.55749764652046E-5));
#26782=DIRECTION('',(-6.12323404134149E-17,1.,-3.14444500472474E-32));
#26783=DIRECTION('axis',(0.,0.,1.));
#26784=DIRECTION('refdir',(1.,0.,0.));
#26785=DIRECTION('center_axis',(0.,-1.,0.));
#26786=DIRECTION('ref_axis',(0.479079334165908,0.,0.877771605587211));
#26787=DIRECTION('center_axis',(0.,1.,0.));
#26788=DIRECTION('ref_axis',(0.479079334179906,0.,0.877771605579571));
#26789=DIRECTION('',(0.,-1.,0.));
#26790=DIRECTION('center_axis',(0.,-1.,0.));
#26791=DIRECTION('ref_axis',(0.479079334179906,0.,0.877771605579571));
#26792=DIRECTION('',(0.,1.,0.));
#26793=DIRECTION('center_axis',(0.,-1.,0.));
#26794=DIRECTION('ref_axis',(0.956725679001188,0.,0.290991366091359));
#26795=DIRECTION('center_axis',(0.,-1.,0.));
#26796=DIRECTION('ref_axis',(0.956725679001044,0.,0.290991366091832));
#26797=DIRECTION('',(0.,1.,0.));
#26798=DIRECTION('center_axis',(0.,1.,0.));
#26799=DIRECTION('ref_axis',(0.956725679001044,0.,0.290991366091832));
#26800=DIRECTION('center_axis',(0.,-1.,0.));
#26801=DIRECTION('ref_axis',(0.853780676609416,0.,-0.520632842076226));
#26802=DIRECTION('center_axis',(0.,1.,0.));
#26803=DIRECTION('ref_axis',(0.853780676602478,0.,-0.520632842087603));
#26804=DIRECTION('',(0.,-1.,0.));
#26805=DIRECTION('center_axis',(0.,-1.,0.));
#26806=DIRECTION('ref_axis',(0.853780676602478,0.,-0.520632842087603));
#26807=DIRECTION('center_axis',(0.22635692418354,0.,-0.974044425513625));
#26808=DIRECTION('ref_axis',(0.,-1.,0.));
#26809=DIRECTION('',(0.974044425513455,0.,0.226356924184268));
#26810=DIRECTION('',(0.,1.,0.));
#26811=DIRECTION('',(-0.974044425513455,0.,-0.226356924184268));
#26812=DIRECTION('center_axis',(0.,-1.,0.));
#26813=DIRECTION('ref_axis',(0.589552929365364,0.,0.80772974655928));
#26814=DIRECTION('center_axis',(0.,1.,0.));
#26815=DIRECTION('ref_axis',(0.589552929372413,0.,0.807729746554134));
#26816=DIRECTION('',(0.,-1.,0.));
#26817=DIRECTION('center_axis',(0.,-1.,0.));
#26818=DIRECTION('ref_axis',(0.589552929372413,0.,0.807729746554134));
#26819=DIRECTION('',(0.,1.,0.));
#26820=DIRECTION('center_axis',(0.,-1.,0.));
#26821=DIRECTION('ref_axis',(0.986522753174914,0.,0.163624134736254));
#26822=DIRECTION('center_axis',(0.,-1.,0.));
#26823=DIRECTION('ref_axis',(0.986522753174814,0.,0.163624134736857));
#26824=DIRECTION('',(0.,1.,0.));
#26825=DIRECTION('center_axis',(0.,1.,0.));
#26826=DIRECTION('ref_axis',(0.986522753174814,0.,0.163624134736857));
#26827=DIRECTION('center_axis',(0.,-1.,0.));
#26828=DIRECTION('ref_axis',(0.778520242143747,0.,-0.627619496647803));
#26829=DIRECTION('center_axis',(0.,1.,0.));
#26830=DIRECTION('ref_axis',(0.778520242139959,0.,-0.627619496652502));
#26831=DIRECTION('',(0.,-1.,0.));
#26832=DIRECTION('center_axis',(0.,-1.,0.));
#26833=DIRECTION('ref_axis',(0.778520242139959,0.,-0.627619496652502));
#26834=DIRECTION('center_axis',(0.0972820994026908,0.,-0.995256847821609));
#26835=DIRECTION('ref_axis',(0.,-1.,0.));
#26836=DIRECTION('',(0.995256847821521,0.,0.0972820994035846));
#26837=DIRECTION('',(0.,1.,0.));
#26838=DIRECTION('',(-0.995256847821521,0.,-0.0972820994035846));
#26839=DIRECTION('center_axis',(0.,-1.,0.));
#26840=DIRECTION('ref_axis',(0.689939110488415,0.,0.723867407622732));
#26841=DIRECTION('center_axis',(0.,1.,0.));
#26842=DIRECTION('ref_axis',(0.689939110489398,0.,0.723867407621795));
#26843=DIRECTION('',(0.,-1.,0.));
#26844=DIRECTION('center_axis',(0.,-1.,0.));
#26845=DIRECTION('ref_axis',(0.689939110489398,0.,0.723867407621795));
#26846=DIRECTION('',(0.,1.,0.));
#26847=DIRECTION('center_axis',(0.,-1.,0.));
#26848=DIRECTION('ref_axis',(0.999440149526036,0.,0.033457249070632));
#26849=DIRECTION('center_axis',(0.,-1.,0.));
#26850=DIRECTION('ref_axis',(0.999440149526012,0.,0.0334572490713498));
#26851=DIRECTION('',(0.,1.,0.));
#26852=DIRECTION('center_axis',(0.,1.,0.));
#26853=DIRECTION('ref_axis',(0.999440149526012,0.,0.0334572490713498));
#26854=DIRECTION('center_axis',(0.,-1.,0.));
#26855=DIRECTION('ref_axis',(0.689939110488415,0.,-0.723867407622732));
#26856=DIRECTION('center_axis',(0.,1.,0.));
#26857=DIRECTION('ref_axis',(0.689939110489398,0.,-0.723867407621795));
#26858=DIRECTION('',(0.,-1.,0.));
#26859=DIRECTION('center_axis',(0.,-1.,0.));
#26860=DIRECTION('ref_axis',(0.689939110489398,0.,-0.723867407621795));
#26861=DIRECTION('center_axis',(-0.0334572490706319,0.,-0.999440149526036));
#26862=DIRECTION('ref_axis',(-0.999440149526036,0.,0.0334572490706319));
#26863=DIRECTION('',(0.999440149526004,0.,-0.0334572490715974));
#26864=DIRECTION('',(0.,1.,0.));
#26865=DIRECTION('',(-0.999440149526004,0.,0.0334572490715974));
#26866=DIRECTION('center_axis',(0.,-1.,0.));
#26867=DIRECTION('ref_axis',(0.778520242143747,0.,0.627619496647803));
#26868=DIRECTION('center_axis',(0.,1.,0.));
#26869=DIRECTION('ref_axis',(0.778520242139959,0.,0.627619496652502));
#26870=DIRECTION('',(0.,-1.,0.));
#26871=DIRECTION('center_axis',(0.,-1.,0.));
#26872=DIRECTION('ref_axis',(0.778520242139959,0.,0.627619496652502));
#26873=DIRECTION('',(0.,1.,0.));
#26874=DIRECTION('center_axis',(0.,-1.,0.));
#26875=DIRECTION('ref_axis',(0.995256847821609,0.,-0.0972820994026908));
#26876=DIRECTION('center_axis',(0.,-1.,0.));
#26877=DIRECTION('ref_axis',(0.995256847821544,0.,-0.0972820994033552));
#26878=DIRECTION('',(0.,1.,0.));
#26879=DIRECTION('center_axis',(0.,1.,0.));
#26880=DIRECTION('ref_axis',(0.995256847821544,0.,-0.0972820994033552));
#26881=DIRECTION('center_axis',(0.,-1.,0.));
#26882=DIRECTION('ref_axis',(0.589552929365356,0.,-0.807729746559286));
#26883=DIRECTION('center_axis',(0.,1.,0.));
#26884=DIRECTION('ref_axis',(0.589552929372405,0.,-0.807729746554141));
#26885=DIRECTION('',(0.,-1.,0.));
#26886=DIRECTION('center_axis',(0.,-1.,0.));
#26887=DIRECTION('ref_axis',(0.589552929372405,0.,-0.807729746554141));
#26888=DIRECTION('center_axis',(-0.163624134736254,0.,-0.986522753174914));
#26889=DIRECTION('ref_axis',(-0.986522753174914,0.,0.163624134736254));
#26890=DIRECTION('',(0.986522753174779,0.,-0.163624134737066));
#26891=DIRECTION('',(0.,1.,0.));
#26892=DIRECTION('',(-0.986522753174779,0.,0.163624134737066));
#26893=DIRECTION('center_axis',(0.,-1.,0.));
#26894=DIRECTION('ref_axis',(0.853780676609419,0.,0.520632842076221));
#26895=DIRECTION('center_axis',(0.,1.,0.));
#26896=DIRECTION('ref_axis',(0.853780676602481,0.,0.520632842087598));
#26897=DIRECTION('',(0.,-1.,0.));
#26898=DIRECTION('center_axis',(0.,-1.,0.));
#26899=DIRECTION('ref_axis',(0.853780676602481,0.,0.520632842087598));
#26900=DIRECTION('',(0.,1.,0.));
#26901=DIRECTION('center_axis',(0.,-1.,0.));
#26902=DIRECTION('ref_axis',(0.974044425513625,0.,-0.22635692418354));
#26903=DIRECTION('center_axis',(0.,-1.,0.));
#26904=DIRECTION('ref_axis',(0.974044425513499,0.,-0.226356924184081));
#26905=DIRECTION('',(0.,1.,0.));
#26906=DIRECTION('center_axis',(0.,1.,0.));
#26907=DIRECTION('ref_axis',(0.974044425513499,0.,-0.226356924184081));
#26908=DIRECTION('center_axis',(0.,-1.,0.));
#26909=DIRECTION('ref_axis',(0.479079334165907,0.,-0.877771605587212));
#26910=DIRECTION('center_axis',(0.,1.,0.));
#26911=DIRECTION('ref_axis',(0.479079334179906,0.,-0.877771605579571));
#26912=DIRECTION('',(0.,-1.,0.));
#26913=DIRECTION('center_axis',(0.,-1.,0.));
#26914=DIRECTION('ref_axis',(0.479079334179906,0.,-0.877771605579571));
#26915=DIRECTION('center_axis',(-0.290991366091359,0.,-0.956725679001188));
#26916=DIRECTION('ref_axis',(-0.956725679001188,0.,0.290991366091359));
#26917=DIRECTION('',(0.956725679000994,0.,-0.290991366091996));
#26918=DIRECTION('',(0.,1.,0.));
#26919=DIRECTION('',(-0.956725679000994,0.,0.290991366091996));
#26920=DIRECTION('center_axis',(0.22635692418354,0.,0.974044425513625));
#26921=DIRECTION('ref_axis',(0.,-1.,0.));
#26922=DIRECTION('',(0.974044425513455,0.,-0.226356924184268));
#26923=DIRECTION('',(0.,-1.,0.));
#26924=DIRECTION('',(-0.974044425513455,0.,0.226356924184268));
#26925=DIRECTION('center_axis',(0.0972820994026909,0.,0.995256847821609));
#26926=DIRECTION('ref_axis',(0.,-1.,0.));
#26927=DIRECTION('',(0.995256847821521,0.,-0.0972820994035846));
#26928=DIRECTION('',(0.,-1.,0.));
#26929=DIRECTION('',(-0.995256847821521,0.,0.0972820994035846));
#26930=DIRECTION('center_axis',(-0.163624134736254,0.,0.986522753174914));
#26931=DIRECTION('ref_axis',(0.,1.,0.));
#26932=DIRECTION('',(0.986522753174779,0.,0.163624134737066));
#26933=DIRECTION('',(0.,-1.,0.));
#26934=DIRECTION('',(-0.986522753174779,0.,-0.163624134737066));
#26935=DIRECTION('center_axis',(-0.290991366091359,0.,0.956725679001188));
#26936=DIRECTION('ref_axis',(0.,1.,0.));
#26937=DIRECTION('',(0.956725679000994,0.,0.290991366091996));
#26938=DIRECTION('',(0.,-1.,0.));
#26939=DIRECTION('',(-0.956725679000994,0.,-0.290991366091996));
#26940=DIRECTION('center_axis',(0.,1.,0.));
#26941=DIRECTION('ref_axis',(-0.942641491092178,0.,-0.333806859233771));
#26942=DIRECTION('center_axis',(0.,-1.,0.));
#26943=DIRECTION('ref_axis',(-0.942641491092022,0.,-0.333806859234212));
#26944=DIRECTION('',(0.,-1.,0.));
#26945=DIRECTION('center_axis',(0.,1.,0.));
#26946=DIRECTION('ref_axis',(-0.942641491092022,0.,-0.333806859234212));
#26947=DIRECTION('center_axis',(0.,1.,0.));
#26948=DIRECTION('ref_axis',(-0.942641491092178,0.,-0.333806859233771));
#26949=DIRECTION('center_axis',(0.,1.,0.));
#26950=DIRECTION('ref_axis',(-0.942641491092022,0.,-0.333806859234212));
#26951=DIRECTION('center_axis',(0.,-1.,0.));
#26952=DIRECTION('ref_axis',(-0.942641491092022,0.,-0.333806859234212));
#26953=DIRECTION('center_axis',(0.,1.,0.));
#26954=DIRECTION('ref_axis',(1.,0.,0.));
#26955=DIRECTION('',(0.942641491091974,0.,-0.333806859234347));
#26956=DIRECTION('center_axis',(0.,-1.,0.));
#26957=DIRECTION('ref_axis',(0.942641491092032,0.,0.333806859234184));
#26958=DIRECTION('',(-0.942641491091975,0.,-0.333806859234346));
#26959=DIRECTION('center_axis',(0.,1.,0.));
#26960=DIRECTION('ref_axis',(-0.942641491092022,0.,-0.333806859234212));
#26961=DIRECTION('center_axis',(0.,1.,0.));
#26962=DIRECTION('ref_axis',(-0.942641491092022,0.,-0.333806859234212));
#26963=DIRECTION('center_axis',(0.,1.,0.));
#26964=DIRECTION('ref_axis',(-0.942641491092022,0.,-0.333806859234212));
#26965=DIRECTION('',(0.999440149526004,0.,0.0334572490715974));
#26966=DIRECTION('center_axis',(0.,1.,0.));
#26967=DIRECTION('ref_axis',(-0.942641491092022,0.,-0.333806859234212));
#26968=DIRECTION('center_axis',(0.,1.,0.));
#26969=DIRECTION('ref_axis',(-0.942641491092178,0.,-0.333806859233771));
#26970=DIRECTION('center_axis',(0.,-1.,0.));
#26971=DIRECTION('ref_axis',(-0.942641491092022,0.,-0.333806859234212));
#26972=DIRECTION('',(0.,-1.,0.));
#26973=DIRECTION('center_axis',(0.,1.,0.));
#26974=DIRECTION('ref_axis',(-0.942641491092178,0.,-0.333806859233771));
#26975=DIRECTION('',(0.,1.,0.));
#26976=DIRECTION('center_axis',(0.,-1.,0.));
#26977=DIRECTION('ref_axis',(-0.942641491092022,0.,-0.333806859234212));
#26978=DIRECTION('center_axis',(-0.0334572490706319,0.,0.999440149526036));
#26979=DIRECTION('ref_axis',(0.,1.,0.));
#26980=DIRECTION('',(-0.999440149526004,0.,-0.0334572490715974));
#26981=DIRECTION('center_axis',(0.,1.,0.));
#26982=DIRECTION('ref_axis',(-0.942641491092178,0.,-0.333806859233771));
#26983=DIRECTION('center_axis',(0.,-1.,0.));
#26984=DIRECTION('ref_axis',(-0.942641491092022,0.,-0.333806859234212));
#26985=DIRECTION('center_axis',(-0.333806859233773,0.,-0.942641491092178));
#26986=DIRECTION('ref_axis',(-0.942641491092178,0.,0.333806859233773));
#26987=DIRECTION('',(-0.942641491091974,0.,0.333806859234347));
#26988=DIRECTION('',(0.,1.,0.));
#26989=DIRECTION('center_axis',(0.,1.,0.));
#26990=DIRECTION('ref_axis',(0.942641491092178,0.,0.333806859233771));
#26991=DIRECTION('center_axis',(0.,1.,0.));
#26992=DIRECTION('ref_axis',(0.942641491092032,0.,0.333806859234184));
#26993=DIRECTION('',(0.,1.,0.));
#26994=DIRECTION('center_axis',(-0.333806859233772,0.,0.942641491092178));
#26995=DIRECTION('ref_axis',(0.,1.,0.));
#26996=DIRECTION('',(0.942641491091975,0.,0.333806859234346));
#26997=DIRECTION('center_axis',(0.,1.,0.));
#26998=DIRECTION('ref_axis',(-0.942641491092178,0.,-0.333806859233771));
#26999=DIRECTION('center_axis',(0.,-1.,0.));
#27000=DIRECTION('ref_axis',(-0.942641491092022,0.,-0.333806859234212));
#27001=DIRECTION('center_axis',(0.,1.,0.));
#27002=DIRECTION('ref_axis',(1.,0.,0.));
#27003=DIRECTION('axis',(0.,0.,1.));
#27004=DIRECTION('refdir',(1.,0.,0.));
#27005=DIRECTION('center_axis',(1.,5.1420277733694E-16,-1.0522467400333E-14));
#27006=DIRECTION('ref_axis',(-1.0522467400333E-14,1.06077175752244E-14,
-1.));
#27007=DIRECTION('',(-1.00001914094642E-12,1.00002200370999E-12,1.));
#27008=DIRECTION('',(-9.47915311079142E-15,-1.,1.E-14));
#27009=DIRECTION('',(1.00001914094642E-12,-9.99999999998997E-13,-1.));
#27010=DIRECTION('',(-9.47915311079142E-15,-1.,1.E-14));
#27011=DIRECTION('center_axis',(1.,5.2084688920845E-16,-1.0522467400333E-14));
#27012=DIRECTION('ref_axis',(-1.0522467400333E-14,1.01548957588061E-14,
-1.));
#27013=DIRECTION('',(-9.56631913100564E-15,9.99999999999985E-15,1.));
#27014=DIRECTION('',(-9.47915311079142E-15,-1.,1.E-14));
#27015=DIRECTION('',(-9.56631913100564E-15,9.99999999999985E-15,1.));
#27016=DIRECTION('',(-9.47915311079142E-15,-1.,1.E-14));
#27017=DIRECTION('center_axis',(-4.5961454925099E-16,1.,6.61092274672771E-17));
#27018=DIRECTION('ref_axis',(-1.05885766278003E-14,6.61092274672722E-17,
-1.));
#27019=DIRECTION('',(1.,-9.54038545074888E-15,9.9999999999998E-15));
#27020=DIRECTION('',(-1.,9.54038545074888E-15,-9.9999999999998E-15));
#27021=DIRECTION('center_axis',(0.,3.71824206197546E-31,1.));
#27022=DIRECTION('ref_axis',(1.,3.89820370584558E-15,-1.44944649852236E-45));
#27023=DIRECTION('center_axis',(-1.99999999991998E-11,2.E-11,1.));
#27024=DIRECTION('ref_axis',(-1.99995712428458E-11,-1.,1.99999999996E-11));
#27025=DIRECTION('',(1.,-9.99466108488984E-13,1.00024333162532E-12));
#27026=DIRECTION('',(-9.99479153109799E-13,-1.,-1.00441888838649E-12));
#27027=DIRECTION('',(1.,-9.99466108488984E-13,1.00024333162532E-12));
#27028=DIRECTION('center_axis',(0.,-4.29362650667545E-31,1.));
#27029=DIRECTION('ref_axis',(4.28756753891971E-16,-1.,-4.29362650667545E-31));
#27030=DIRECTION('',(-9.99999999999976E-15,-1.04336808689941E-14,1.));
#27031=DIRECTION('center_axis',(-1.99999999991998E-11,2.E-11,1.));
#27032=DIRECTION('ref_axis',(-1.99995712428458E-11,-1.,1.99999999996E-11));
#27033=DIRECTION('center_axis',(-1.0522467400333E-14,6.93088260946523E-29,
-1.));
#27034=DIRECTION('ref_axis',(1.,-6.62426369448742E-15,-1.0522467400333E-14));
#27035=DIRECTION('',(-1.,9.99485333130104E-13,-9.99628143109513E-13));
#27036=DIRECTION('',(9.99479153109799E-13,1.,1.00441888838649E-12));
#27037=DIRECTION('',(1.,-9.99466108488984E-13,1.00024333162532E-12));
#27038=DIRECTION('center_axis',(5.33891510011771E-16,-1.,2.20037109950003E-17));
#27039=DIRECTION('ref_axis',(-1.,-5.33891510011771E-16,1.0522467400333E-14));
#27040=DIRECTION('',(9.99999999998993E-13,-1.00002200370999E-12,-1.));
#27041=DIRECTION('center_axis',(-5.3389151001178E-16,1.,6.61092274672815E-17));
#27042=DIRECTION('ref_axis',(-9.50035731417012E-15,6.61092274672764E-17,
-1.));
#27043=DIRECTION('',(-9.99999999998985E-13,-1.00108821931263E-12,1.));
#27044=DIRECTION('center_axis',(1.,5.33891510011885E-16,-1.0522467400333E-14));
#27045=DIRECTION('ref_axis',(-1.0522467400333E-14,1.08319082541355E-14,
-1.));
#27046=DIRECTION('axis',(0.,0.,1.));
#27047=DIRECTION('refdir',(1.,0.,0.));
#27048=DIRECTION('center_axis',(0.,1.,0.));
#27049=DIRECTION('ref_axis',(-0.293165390088848,0.,-0.956061741758373));
#27050=DIRECTION('',(0.,-1.,0.));
#27051=DIRECTION('center_axis',(0.,1.,0.));
#27052=DIRECTION('ref_axis',(-0.293165390092017,0.,-0.956061741757401));
#27053=DIRECTION('',(0.,-1.,0.));
#27054=DIRECTION('center_axis',(0.,-1.,0.));
#27055=DIRECTION('ref_axis',(-0.293165390092017,0.,-0.956061741757401));
#27056=DIRECTION('center_axis',(0.,0.,-1.));
#27057=DIRECTION('ref_axis',(0.,-1.,0.));
#27058=DIRECTION('',(0.,-1.,0.));
#27059=DIRECTION('',(1.,0.,0.));
#27060=DIRECTION('',(-1.,0.,0.));
#27061=DIRECTION('center_axis',(0.,1.,0.));
#27062=DIRECTION('ref_axis',(0.293165390088847,0.,-0.956061741758373));
#27063=DIRECTION('',(0.,-1.,0.));
#27064=DIRECTION('center_axis',(0.,1.,0.));
#27065=DIRECTION('ref_axis',(0.293165390092016,0.,-0.956061741757401));
#27066=DIRECTION('center_axis',(0.,-1.,0.));
#27067=DIRECTION('ref_axis',(0.293165390092016,0.,-0.956061741757401));
#27068=DIRECTION('center_axis',(0.,1.,0.));
#27069=DIRECTION('ref_axis',(0.841791044776119,0.,-0.539803516971434));
#27070=DIRECTION('',(0.,-1.,0.));
#27071=DIRECTION('center_axis',(0.,-1.,0.));
#27072=DIRECTION('ref_axis',(0.841791044776055,0.,-0.539803516971535));
#27073=DIRECTION('center_axis',(0.,1.,0.));
#27074=DIRECTION('ref_axis',(0.841791044776055,0.,-0.539803516971535));
#27075=DIRECTION('center_axis',(0.,1.,0.));
#27076=DIRECTION('ref_axis',(0.956061741758373,0.,-0.293165390088847));
#27077=DIRECTION('',(0.,-1.,0.));
#27078=DIRECTION('center_axis',(0.,1.,0.));
#27079=DIRECTION('ref_axis',(0.956061741757401,0.,-0.293165390092016));
#27080=DIRECTION('center_axis',(0.,-1.,0.));
#27081=DIRECTION('ref_axis',(0.956061741757401,0.,-0.293165390092016));
#27082=DIRECTION('center_axis',(1.,2.68038322042824E-32,4.38829015768159E-48));
#27083=DIRECTION('ref_axis',(3.64629801437176E-63,-1.63718759475762E-16,
1.));
#27084=DIRECTION('',(0.,-1.,0.));
#27085=DIRECTION('',(-1.00016371875848E-12,0.,1.));
#27086=DIRECTION('',(1.00016371875848E-12,0.,-1.));
#27087=DIRECTION('center_axis',(0.,1.,0.));
#27088=DIRECTION('ref_axis',(0.956061741758373,0.,0.293165390088847));
#27089=DIRECTION('',(0.,-1.,0.));
#27090=DIRECTION('center_axis',(0.,1.,0.));
#27091=DIRECTION('ref_axis',(0.956061741757401,0.,0.293165390092016));
#27092=DIRECTION('center_axis',(0.,-1.,0.));
#27093=DIRECTION('ref_axis',(0.956061741757401,0.,0.293165390092016));
#27094=DIRECTION('center_axis',(0.,1.,0.));
#27095=DIRECTION('ref_axis',(0.539803516971435,0.,0.841791044776119));
#27096=DIRECTION('',(0.,1.,0.));
#27097=DIRECTION('center_axis',(0.,-1.,0.));
#27098=DIRECTION('ref_axis',(0.539803516971536,0.,0.841791044776054));
#27099=DIRECTION('center_axis',(0.,1.,0.));
#27100=DIRECTION('ref_axis',(0.539803516971536,0.,0.841791044776054));
#27101=DIRECTION('center_axis',(0.,1.,0.));
#27102=DIRECTION('ref_axis',(-0.956061741758373,0.,-0.293165390088847));
#27103=DIRECTION('',(0.,-1.,0.));
#27104=DIRECTION('center_axis',(0.,1.,0.));
#27105=DIRECTION('ref_axis',(-0.956061741757401,0.,-0.293165390092016));
#27106=DIRECTION('',(0.,-1.,0.));
#27107=DIRECTION('center_axis',(0.,-1.,0.));
#27108=DIRECTION('ref_axis',(-0.956061741757401,0.,-0.293165390092016));
#27109=DIRECTION('center_axis',(-1.,0.,0.));
#27110=DIRECTION('ref_axis',(0.,0.,1.));
#27111=DIRECTION('',(0.,0.,-1.));
#27112=DIRECTION('',(0.,-1.,0.));
#27113=DIRECTION('',(0.,0.,1.));
#27114=DIRECTION('center_axis',(0.,-1.,0.));
#27115=DIRECTION('ref_axis',(-0.956061741758373,0.,0.293165390088847));
#27116=DIRECTION('center_axis',(0.,1.,0.));
#27117=DIRECTION('ref_axis',(-0.956061741757401,0.,0.293165390092016));
#27118=DIRECTION('',(0.,-1.,0.));
#27119=DIRECTION('center_axis',(0.,-1.,0.));
#27120=DIRECTION('ref_axis',(-0.956061741757401,0.,0.293165390092016));
#27121=DIRECTION('center_axis',(0.,1.,0.));
#27122=DIRECTION('ref_axis',(-0.841791044776119,0.,0.539803516971435));
#27123=DIRECTION('center_axis',(0.,-1.,0.));
#27124=DIRECTION('ref_axis',(-0.841791044776054,0.,0.539803516971536));
#27125=DIRECTION('',(0.,-1.,0.));
#27126=DIRECTION('center_axis',(0.,1.,0.));
#27127=DIRECTION('ref_axis',(-0.841791044776054,0.,0.539803516971536));
#27128=DIRECTION('center_axis',(0.,1.,0.));
#27129=DIRECTION('ref_axis',(-0.293165390088847,0.,0.956061741758373));
#27130=DIRECTION('center_axis',(0.,1.,0.));
#27131=DIRECTION('ref_axis',(-0.293165390092016,0.,0.956061741757401));
#27132=DIRECTION('',(0.,-1.,0.));
#27133=DIRECTION('center_axis',(0.,-1.,0.));
#27134=DIRECTION('ref_axis',(-0.293165390092016,0.,0.956061741757401));
#27135=DIRECTION('center_axis',(0.,0.,1.));
#27136=DIRECTION('ref_axis',(1.,0.,0.));
#27137=DIRECTION('',(-1.,0.,0.));
#27138=DIRECTION('',(0.,-1.,0.));
#27139=DIRECTION('',(1.,0.,0.));
#27140=DIRECTION('center_axis',(0.,1.,0.));
#27141=DIRECTION('ref_axis',(0.293165390088847,0.,0.956061741758373));
#27142=DIRECTION('center_axis',(0.,1.,0.));
#27143=DIRECTION('ref_axis',(0.293165390092016,0.,0.956061741757401));
#27144=DIRECTION('center_axis',(0.,-1.,0.));
#27145=DIRECTION('ref_axis',(0.293165390092016,0.,0.956061741757401));
#27146=DIRECTION('center_axis',(0.,1.,0.));
#27147=DIRECTION('ref_axis',(1.,0.,0.));
#27148=DIRECTION('center_axis',(0.,-1.,0.));
#27149=DIRECTION('ref_axis',(-0.539803516971535,0.,-0.841791044776055));
#27150=DIRECTION('center_axis',(0.,1.,0.));
#27151=DIRECTION('ref_axis',(1.,0.,0.));
#27152=DIRECTION('center_axis',(0.,1.,0.));
#27153=DIRECTION('ref_axis',(1.,0.,0.));
#27154=DIRECTION('center_axis',(0.,1.,0.));
#27155=DIRECTION('ref_axis',(1.,0.,0.));
#27156=DIRECTION('center_axis',(0.,1.,0.));
#27157=DIRECTION('ref_axis',(1.,0.,0.));
#27158=DIRECTION('',(0.707106781186548,0.,0.707106781186547));
#27159=DIRECTION('',(1.,0.,-1.00027992850901E-12));
#27160=DIRECTION('',(0.707106781186547,0.,-0.707106781186548));
#27161=DIRECTION('',(-1.000139964254E-12,0.,-1.));
#27162=DIRECTION('',(-0.707106781186548,0.,-0.707106781186547));
#27163=DIRECTION('',(-1.,0.,1.000139964254E-12));
#27164=DIRECTION('',(-0.707106781186547,0.,0.707106781186548));
#27165=DIRECTION('',(1.000139964254E-12,0.,1.));
#27166=DIRECTION('center_axis',(0.,1.,0.));
#27167=DIRECTION('ref_axis',(-0.539803516971434,0.,-0.841791044776119));
#27168=DIRECTION('center_axis',(0.,1.,0.));
#27169=DIRECTION('ref_axis',(-0.539803516971535,0.,-0.841791044776055));
#27170=DIRECTION('center_axis',(0.,1.,0.));
#27171=DIRECTION('ref_axis',(1.,0.,0.));
#27172=DIRECTION('',(0.,1.,0.));
#27173=DIRECTION('center_axis',(0.,-1.,0.));
#27174=DIRECTION('ref_axis',(1.,0.,0.));
#27175=DIRECTION('center_axis',(0.,1.,0.));
#27176=DIRECTION('ref_axis',(1.,0.,0.));
#27177=DIRECTION('',(0.,1.,0.));
#27178=DIRECTION('center_axis',(0.,-1.,0.));
#27179=DIRECTION('ref_axis',(1.,0.,0.));
#27180=DIRECTION('center_axis',(0.,1.,0.));
#27181=DIRECTION('ref_axis',(1.,0.,0.));
#27182=DIRECTION('',(0.,1.,0.));
#27183=DIRECTION('center_axis',(0.,-1.,0.));
#27184=DIRECTION('ref_axis',(1.,0.,0.));
#27185=DIRECTION('center_axis',(0.,1.,0.));
#27186=DIRECTION('ref_axis',(1.,0.,0.));
#27187=DIRECTION('',(0.,1.,0.));
#27188=DIRECTION('center_axis',(0.,-1.,0.));
#27189=DIRECTION('ref_axis',(1.,0.,0.));
#27190=DIRECTION('center_axis',(-2.79928510006155E-16,0.,-1.));
#27191=DIRECTION('ref_axis',(-1.,0.,2.79928510006155E-16));
#27192=DIRECTION('',(0.,-1.,0.));
#27193=DIRECTION('',(-1.,0.,1.00027992850901E-12));
#27194=DIRECTION('',(0.,1.,0.));
#27195=DIRECTION('center_axis',(-0.707106781186548,0.,-0.707106781186547));
#27196=DIRECTION('ref_axis',(-0.707106781186547,0.,0.707106781186548));
#27197=DIRECTION('',(-0.707106781186547,0.,0.707106781186548));
#27198=DIRECTION('',(0.,1.,0.));
#27199=DIRECTION('center_axis',(-1.,0.,1.39964255003077E-16));
#27200=DIRECTION('ref_axis',(0.,1.,0.));
#27201=DIRECTION('',(1.000139964254E-12,0.,1.));
#27202=DIRECTION('',(0.,1.,0.));
#27203=DIRECTION('center_axis',(-0.707106781186547,0.,0.707106781186548));
#27204=DIRECTION('ref_axis',(0.,1.,0.));
#27205=DIRECTION('',(0.707106781186548,0.,0.707106781186547));
#27206=DIRECTION('',(0.,1.,0.));
#27207=DIRECTION('center_axis',(2.74189873077128E-48,1.95899926785664E-32,
1.));
#27208=DIRECTION('ref_axis',(1.,-1.39964255003077E-16,-7.02611785152007E-64));
#27209=DIRECTION('',(1.,0.,-1.000139964254E-12));
#27210=DIRECTION('',(0.,1.,0.));
#27211=DIRECTION('center_axis',(0.707106781186548,0.,0.707106781186547));
#27212=DIRECTION('ref_axis',(0.,-1.,0.));
#27213=DIRECTION('',(0.707106781186547,0.,-0.707106781186548));
#27214=DIRECTION('',(0.,1.,0.));
#27215=DIRECTION('center_axis',(1.,0.,-1.39964255003077E-16));
#27216=DIRECTION('ref_axis',(0.,1.,0.));
#27217=DIRECTION('',(-1.000139964254E-12,0.,-1.));
#27218=DIRECTION('',(0.,1.,0.));
#27219=DIRECTION('center_axis',(0.707106781186547,0.,-0.707106781186548));
#27220=DIRECTION('ref_axis',(0.,-1.,0.));
#27221=DIRECTION('',(-0.707106781186548,0.,-0.707106781186547));
#27222=DIRECTION('center_axis',(0.,1.,0.));
#27223=DIRECTION('ref_axis',(1.,0.,0.));
#27224=DIRECTION('axis',(0.,0.,1.));
#27225=DIRECTION('refdir',(1.,0.,0.));
#27226=DIRECTION('center_axis',(0.,-1.,0.));
#27227=DIRECTION('ref_axis',(-0.877771605587211,0.,0.479079334165908));
#27228=DIRECTION('center_axis',(0.,1.,0.));
#27229=DIRECTION('ref_axis',(-0.877771605579571,0.,0.479079334179906));
#27230=DIRECTION('',(0.,-1.,0.));
#27231=DIRECTION('center_axis',(0.,-1.,0.));
#27232=DIRECTION('ref_axis',(-0.877771605579571,0.,0.479079334179906));
#27233=DIRECTION('',(0.,1.,0.));
#27234=DIRECTION('center_axis',(0.,-1.,0.));
#27235=DIRECTION('ref_axis',(-0.290991366091359,0.,0.956725679001188));
#27236=DIRECTION('center_axis',(0.,-1.,0.));
#27237=DIRECTION('ref_axis',(-0.290991366091832,0.,0.956725679001044));
#27238=DIRECTION('',(0.,1.,0.));
#27239=DIRECTION('center_axis',(0.,1.,0.));
#27240=DIRECTION('ref_axis',(-0.290991366091832,0.,0.956725679001044));
#27241=DIRECTION('center_axis',(0.,-1.,0.));
#27242=DIRECTION('ref_axis',(0.520632842076226,0.,0.853780676609416));
#27243=DIRECTION('center_axis',(0.,1.,0.));
#27244=DIRECTION('ref_axis',(0.520632842087603,0.,0.853780676602478));
#27245=DIRECTION('',(0.,-1.,0.));
#27246=DIRECTION('center_axis',(0.,-1.,0.));
#27247=DIRECTION('ref_axis',(0.520632842087603,0.,0.853780676602478));
#27248=DIRECTION('center_axis',(0.974044425513625,0.,0.22635692418354));
#27249=DIRECTION('ref_axis',(0.,-1.,0.));
#27250=DIRECTION('',(-0.226356924184268,0.,0.974044425513455));
#27251=DIRECTION('',(0.,1.,0.));
#27252=DIRECTION('',(0.226356924184268,0.,-0.974044425513455));
#27253=DIRECTION('center_axis',(0.,-1.,0.));
#27254=DIRECTION('ref_axis',(-0.80772974655928,0.,0.589552929365364));
#27255=DIRECTION('center_axis',(0.,1.,0.));
#27256=DIRECTION('ref_axis',(-0.807729746554134,0.,0.589552929372413));
#27257=DIRECTION('',(0.,-1.,0.));
#27258=DIRECTION('center_axis',(0.,-1.,0.));
#27259=DIRECTION('ref_axis',(-0.807729746554134,0.,0.589552929372413));
#27260=DIRECTION('',(0.,1.,0.));
#27261=DIRECTION('center_axis',(0.,-1.,0.));
#27262=DIRECTION('ref_axis',(-0.163624134736254,0.,0.986522753174914));
#27263=DIRECTION('center_axis',(0.,-1.,0.));
#27264=DIRECTION('ref_axis',(-0.163624134736857,0.,0.986522753174814));
#27265=DIRECTION('',(0.,1.,0.));
#27266=DIRECTION('center_axis',(0.,1.,0.));
#27267=DIRECTION('ref_axis',(-0.163624134736857,0.,0.986522753174814));
#27268=DIRECTION('center_axis',(0.,-1.,0.));
#27269=DIRECTION('ref_axis',(0.627619496647803,0.,0.778520242143747));
#27270=DIRECTION('center_axis',(0.,1.,0.));
#27271=DIRECTION('ref_axis',(0.627619496652502,0.,0.778520242139959));
#27272=DIRECTION('',(0.,-1.,0.));
#27273=DIRECTION('center_axis',(0.,-1.,0.));
#27274=DIRECTION('ref_axis',(0.627619496652502,0.,0.778520242139959));
#27275=DIRECTION('center_axis',(0.995256847821609,0.,0.0972820994026908));
#27276=DIRECTION('ref_axis',(0.,-1.,0.));
#27277=DIRECTION('',(-0.0972820994035846,0.,0.995256847821521));
#27278=DIRECTION('',(0.,1.,0.));
#27279=DIRECTION('',(0.0972820994035846,0.,-0.995256847821521));
#27280=DIRECTION('center_axis',(0.,-1.,0.));
#27281=DIRECTION('ref_axis',(-0.723867407622732,0.,0.689939110488415));
#27282=DIRECTION('center_axis',(0.,1.,0.));
#27283=DIRECTION('ref_axis',(-0.723867407621795,0.,0.689939110489398));
#27284=DIRECTION('',(0.,-1.,0.));
#27285=DIRECTION('center_axis',(0.,-1.,0.));
#27286=DIRECTION('ref_axis',(-0.723867407621795,0.,0.689939110489398));
#27287=DIRECTION('',(0.,1.,0.));
#27288=DIRECTION('center_axis',(0.,-1.,0.));
#27289=DIRECTION('ref_axis',(-0.033457249070632,0.,0.999440149526036));
#27290=DIRECTION('center_axis',(0.,-1.,0.));
#27291=DIRECTION('ref_axis',(-0.0334572490713498,0.,0.999440149526012));
#27292=DIRECTION('',(0.,1.,0.));
#27293=DIRECTION('center_axis',(0.,1.,0.));
#27294=DIRECTION('ref_axis',(-0.0334572490713498,0.,0.999440149526012));
#27295=DIRECTION('center_axis',(0.,-1.,0.));
#27296=DIRECTION('ref_axis',(0.723867407622732,0.,0.689939110488415));
#27297=DIRECTION('center_axis',(0.,1.,0.));
#27298=DIRECTION('ref_axis',(0.723867407621795,0.,0.689939110489398));
#27299=DIRECTION('',(0.,-1.,0.));
#27300=DIRECTION('center_axis',(0.,-1.,0.));
#27301=DIRECTION('ref_axis',(0.723867407621795,0.,0.689939110489398));
#27302=DIRECTION('center_axis',(0.999440149526036,0.,-0.0334572490706319));
#27303=DIRECTION('ref_axis',(0.,-1.,0.));
#27304=DIRECTION('',(0.0334572490715974,0.,0.999440149526004));
#27305=DIRECTION('',(0.,1.,0.));
#27306=DIRECTION('',(-0.0334572490715974,0.,-0.999440149526004));
#27307=DIRECTION('center_axis',(0.,-1.,0.));
#27308=DIRECTION('ref_axis',(-0.627619496647803,0.,0.778520242143747));
#27309=DIRECTION('center_axis',(0.,1.,0.));
#27310=DIRECTION('ref_axis',(-0.627619496652502,0.,0.778520242139959));
#27311=DIRECTION('',(0.,-1.,0.));
#27312=DIRECTION('center_axis',(0.,-1.,0.));
#27313=DIRECTION('ref_axis',(-0.627619496652502,0.,0.778520242139959));
#27314=DIRECTION('',(0.,1.,0.));
#27315=DIRECTION('center_axis',(0.,-1.,0.));
#27316=DIRECTION('ref_axis',(0.0972820994026908,0.,0.995256847821609));
#27317=DIRECTION('center_axis',(0.,-1.,0.));
#27318=DIRECTION('ref_axis',(0.0972820994033552,0.,0.995256847821544));
#27319=DIRECTION('',(0.,1.,0.));
#27320=DIRECTION('center_axis',(0.,1.,0.));
#27321=DIRECTION('ref_axis',(0.0972820994033552,0.,0.995256847821544));
#27322=DIRECTION('center_axis',(0.,-1.,0.));
#27323=DIRECTION('ref_axis',(0.807729746559285,0.,0.589552929365357));
#27324=DIRECTION('center_axis',(0.,1.,0.));
#27325=DIRECTION('ref_axis',(0.80772974655414,0.,0.589552929372406));
#27326=DIRECTION('',(0.,-1.,0.));
#27327=DIRECTION('center_axis',(0.,-1.,0.));
#27328=DIRECTION('ref_axis',(0.80772974655414,0.,0.589552929372406));
#27329=DIRECTION('center_axis',(0.986522753174914,0.,-0.163624134736254));
#27330=DIRECTION('ref_axis',(0.,-1.,0.));
#27331=DIRECTION('',(0.163624134737066,0.,0.986522753174779));
#27332=DIRECTION('',(0.,1.,0.));
#27333=DIRECTION('',(-0.163624134737066,0.,-0.986522753174779));
#27334=DIRECTION('center_axis',(0.,-1.,0.));
#27335=DIRECTION('ref_axis',(-0.520632842076221,0.,0.853780676609419));
#27336=DIRECTION('center_axis',(0.,1.,0.));
#27337=DIRECTION('ref_axis',(-0.520632842087598,0.,0.853780676602481));
#27338=DIRECTION('',(0.,-1.,0.));
#27339=DIRECTION('center_axis',(0.,-1.,0.));
#27340=DIRECTION('ref_axis',(-0.520632842087598,0.,0.853780676602481));
#27341=DIRECTION('',(0.,1.,0.));
#27342=DIRECTION('center_axis',(0.,-1.,0.));
#27343=DIRECTION('ref_axis',(0.22635692418354,0.,0.974044425513625));
#27344=DIRECTION('center_axis',(0.,-1.,0.));
#27345=DIRECTION('ref_axis',(0.226356924184081,0.,0.974044425513499));
#27346=DIRECTION('',(0.,1.,0.));
#27347=DIRECTION('center_axis',(0.,1.,0.));
#27348=DIRECTION('ref_axis',(0.226356924184081,0.,0.974044425513499));
#27349=DIRECTION('center_axis',(0.,-1.,0.));
#27350=DIRECTION('ref_axis',(0.877771605587212,0.,0.479079334165907));
#27351=DIRECTION('center_axis',(0.,1.,0.));
#27352=DIRECTION('ref_axis',(0.877771605579571,0.,0.479079334179906));
#27353=DIRECTION('',(0.,-1.,0.));
#27354=DIRECTION('center_axis',(0.,-1.,0.));
#27355=DIRECTION('ref_axis',(0.877771605579571,0.,0.479079334179906));
#27356=DIRECTION('center_axis',(0.956725679001188,0.,-0.290991366091359));
#27357=DIRECTION('ref_axis',(0.,-1.,0.));
#27358=DIRECTION('',(0.290991366091996,0.,0.956725679000994));
#27359=DIRECTION('',(0.,1.,0.));
#27360=DIRECTION('',(-0.290991366091996,0.,-0.956725679000994));
#27361=DIRECTION('center_axis',(-0.974044425513625,0.,0.22635692418354));
#27362=DIRECTION('ref_axis',(0.,1.,0.));
#27363=DIRECTION('',(0.226356924184268,0.,0.974044425513455));
#27364=DIRECTION('',(0.,-1.,0.));
#27365=DIRECTION('',(-0.226356924184268,0.,-0.974044425513455));
#27366=DIRECTION('center_axis',(-0.995256847821609,0.,0.0972820994026909));
#27367=DIRECTION('ref_axis',(0.,1.,0.));
#27368=DIRECTION('',(0.0972820994035846,0.,0.995256847821521));
#27369=DIRECTION('',(0.,-1.,0.));
#27370=DIRECTION('',(-0.0972820994035846,0.,-0.995256847821521));
#27371=DIRECTION('center_axis',(-0.986522753174914,0.,-0.163624134736254));
#27372=DIRECTION('ref_axis',(-0.163624134736254,0.,0.986522753174914));
#27373=DIRECTION('',(-0.163624134737066,0.,0.986522753174779));
#27374=DIRECTION('',(0.,-1.,0.));
#27375=DIRECTION('',(0.163624134737066,0.,-0.986522753174779));
#27376=DIRECTION('center_axis',(-0.956725679001188,0.,-0.290991366091359));
#27377=DIRECTION('ref_axis',(-0.290991366091359,0.,0.956725679001188));
#27378=DIRECTION('',(-0.290991366091996,0.,0.956725679000994));
#27379=DIRECTION('',(0.,-1.,0.));
#27380=DIRECTION('',(0.290991366091996,0.,-0.956725679000994));
#27381=DIRECTION('center_axis',(0.,1.,0.));
#27382=DIRECTION('ref_axis',(0.333806859233771,0.,-0.942641491092178));
#27383=DIRECTION('center_axis',(0.,-1.,0.));
#27384=DIRECTION('ref_axis',(0.333806859234212,0.,-0.942641491092022));
#27385=DIRECTION('',(0.,1.,0.));
#27386=DIRECTION('center_axis',(0.,1.,0.));
#27387=DIRECTION('ref_axis',(0.333806859234212,0.,-0.942641491092022));
#27388=DIRECTION('center_axis',(0.,1.,0.));
#27389=DIRECTION('ref_axis',(0.333806859233771,0.,-0.942641491092178));
#27390=DIRECTION('center_axis',(0.,1.,0.));
#27391=DIRECTION('ref_axis',(0.333806859234212,0.,-0.942641491092022));
#27392=DIRECTION('center_axis',(0.,-1.,0.));
#27393=DIRECTION('ref_axis',(0.333806859234212,0.,-0.942641491092022));
#27394=DIRECTION('center_axis',(0.,1.,0.));
#27395=DIRECTION('ref_axis',(1.,0.,0.));
#27396=DIRECTION('',(0.333806859234347,0.,0.942641491091974));
#27397=DIRECTION('center_axis',(0.,-1.,0.));
#27398=DIRECTION('ref_axis',(-0.333806859234184,0.,0.942641491092032));
#27399=DIRECTION('',(0.333806859234347,0.,-0.942641491091974));
#27400=DIRECTION('center_axis',(0.,1.,0.));
#27401=DIRECTION('ref_axis',(0.333806859234212,0.,-0.942641491092022));
#27402=DIRECTION('center_axis',(0.,1.,0.));
#27403=DIRECTION('ref_axis',(0.333806859234212,0.,-0.942641491092022));
#27404=DIRECTION('center_axis',(0.,1.,0.));
#27405=DIRECTION('ref_axis',(0.333806859234212,0.,-0.942641491092022));
#27406=DIRECTION('',(-0.0334572490715974,0.,0.999440149526004));
#27407=DIRECTION('center_axis',(0.,1.,0.));
#27408=DIRECTION('ref_axis',(0.333806859234212,0.,-0.942641491092022));
#27409=DIRECTION('center_axis',(0.,1.,0.));
#27410=DIRECTION('ref_axis',(0.333806859233771,0.,-0.942641491092178));
#27411=DIRECTION('center_axis',(0.,-1.,0.));
#27412=DIRECTION('ref_axis',(0.333806859234212,0.,-0.942641491092022));
#27413=DIRECTION('',(0.,-1.,0.));
#27414=DIRECTION('center_axis',(0.,1.,0.));
#27415=DIRECTION('ref_axis',(0.333806859233771,0.,-0.942641491092178));
#27416=DIRECTION('',(0.,1.,0.));
#27417=DIRECTION('center_axis',(0.,-1.,0.));
#27418=DIRECTION('ref_axis',(0.333806859234212,0.,-0.942641491092022));
#27419=DIRECTION('center_axis',(-0.999440149526036,0.,-0.0334572490706319));
#27420=DIRECTION('ref_axis',(-0.0334572490706319,0.,0.999440149526036));
#27421=DIRECTION('',(0.0334572490715974,0.,-0.999440149526004));
#27422=DIRECTION('center_axis',(0.,1.,0.));
#27423=DIRECTION('ref_axis',(0.333806859233771,0.,-0.942641491092178));
#27424=DIRECTION('center_axis',(0.,-1.,0.));
#27425=DIRECTION('ref_axis',(0.333806859234212,0.,-0.942641491092022));
#27426=DIRECTION('center_axis',(0.,1.,0.));
#27427=DIRECTION('ref_axis',(-0.333806859233771,0.,0.942641491092178));
#27428=DIRECTION('',(0.,-1.,0.));
#27429=DIRECTION('center_axis',(0.,1.,0.));
#27430=DIRECTION('ref_axis',(-0.333806859234184,0.,0.942641491092032));
#27431=DIRECTION('',(0.,1.,0.));
#27432=DIRECTION('center_axis',(-0.942641491092178,0.,-0.333806859233773));
#27433=DIRECTION('ref_axis',(-0.333806859233773,0.,0.942641491092178));
#27434=DIRECTION('',(-0.333806859234347,0.,0.942641491091974));
#27435=DIRECTION('center_axis',(0.,1.,0.));
#27436=DIRECTION('ref_axis',(0.333806859233771,0.,-0.942641491092178));
#27437=DIRECTION('center_axis',(0.,-1.,0.));
#27438=DIRECTION('ref_axis',(0.333806859234212,0.,-0.942641491092022));
#27439=DIRECTION('center_axis',(0.942641491092178,0.,-0.333806859233773));
#27440=DIRECTION('ref_axis',(0.,-1.,0.));
#27441=DIRECTION('',(-0.333806859234347,0.,-0.942641491091974));
#27442=DIRECTION('center_axis',(0.,1.,0.));
#27443=DIRECTION('ref_axis',(1.,0.,0.));
#27444=DIRECTION('axis',(0.,0.,1.));
#27445=DIRECTION('refdir',(1.,0.,0.));
#27446=DIRECTION('center_axis',(-5.6420062889325E-16,1.,6.61092274672818E-17));
#27447=DIRECTION('ref_axis',(-9.50035731417012E-15,6.61092274672764E-17,
-1.));
#27448=DIRECTION('',(-1.00001914094641E-12,-1.00108821931263E-12,1.));
#27449=DIRECTION('',(-1.,9.99435799370104E-13,-1.0001463424449E-12));
#27450=DIRECTION('',(9.99999999998985E-13,1.00108821931263E-12,-1.));
#27451=DIRECTION('',(-1.,9.99435799370104E-13,-1.0001463424449E-12));
#27452=DIRECTION('center_axis',(-1.46342445914483E-16,-4.41888838750563E-15,
1.));
#27453=DIRECTION('ref_axis',(1.,3.89820370584558E-15,1.463424459145E-16));
#27454=DIRECTION('',(-9.99485797221669E-13,-1.,-1.00441888838649E-12));
#27455=DIRECTION('',(9.99479153109799E-13,1.,1.00441888838649E-12));
#27456=DIRECTION('',(-1.,9.99435799370104E-13,-1.0001463424449E-12));
#27457=DIRECTION('center_axis',(5.64200628893241E-16,-1.,2.20037109950003E-17));
#27458=DIRECTION('ref_axis',(-1.,-5.64200628893241E-16,1.0522467400333E-14));
#27459=DIRECTION('',(1.00001914094642E-12,-1.00002200370999E-12,-1.));
#27460=DIRECTION('',(-9.99999999998993E-13,1.00002200370999E-12,1.));
#27461=DIRECTION('',(-1.,9.99435799370104E-13,-1.0001463424449E-12));
#27462=DIRECTION('center_axis',(-1.0522467400333E-14,4.4188883875057E-15,
-1.));
#27463=DIRECTION('ref_axis',(1.,-6.77060614040192E-15,-1.0522467400333E-14));
#27464=DIRECTION('',(9.99485797221669E-13,1.,1.00441888838649E-12));
#27465=DIRECTION('',(-9.99479153109799E-13,-1.,-1.00441888838649E-12));
#27466=DIRECTION('center_axis',(-2.79702568992599E-16,2.20037109950002E-17,
1.));
#27467=DIRECTION('ref_axis',(1.,3.89820370584558E-15,2.79702568992599E-16));
#27468=DIRECTION('',(-9.99485797221648E-13,-1.,1.00002200371E-12));
#27469=DIRECTION('',(-1.,9.99435799370104E-13,-1.00027970256798E-12));
#27470=DIRECTION('',(9.99479153109778E-13,1.,-1.00002200371E-12));
#27471=DIRECTION('',(-1.,9.99435799370104E-13,-1.00027970256798E-12));
#27472=DIRECTION('center_axis',(5.64200628893241E-16,-1.,2.20037109950003E-17));
#27473=DIRECTION('ref_axis',(-1.,-5.64200628893241E-16,1.0522467400333E-14));
#27474=DIRECTION('',(1.00001914094642E-12,-1.00002200370999E-12,-1.));
#27475=DIRECTION('',(-9.99999999998993E-13,1.00002200370999E-12,1.));
#27476=DIRECTION('',(-1.,9.99435799370104E-13,-1.00027970256798E-12));
#27477=DIRECTION('center_axis',(-1.0522467400333E-14,-2.20037109949256E-17,
-1.));
#27478=DIRECTION('ref_axis',(1.,-6.90396626348002E-15,-1.0522467400333E-14));
#27479=DIRECTION('',(9.99485797221648E-13,1.,-1.00002200371E-12));
#27480=DIRECTION('',(-9.99479153109778E-13,-1.,1.00002200371E-12));
#27481=DIRECTION('',(-1.,9.99435799370104E-13,-1.00027970256798E-12));
#27482=DIRECTION('center_axis',(-5.6420062889324E-16,1.,6.61092274672781E-17));
#27483=DIRECTION('ref_axis',(-1.06105803387953E-14,6.61092274672721E-17,
-1.));
#27484=DIRECTION('',(-1.00001914094642E-12,1.00002200370999E-12,1.));
#27485=DIRECTION('',(9.99999999998993E-13,-1.00002200370999E-12,-1.));
#27486=DIRECTION('center_axis',(-1.0522467400333E-14,-2.2003710994928E-17,
-1.));
#27487=DIRECTION('ref_axis',(1.,-6.77060614040192E-15,-1.0522467400333E-14));
#27488=DIRECTION('',(9.99485797221648E-13,1.,-1.00002200371E-12));
#27489=DIRECTION('',(-1.,9.99435799370104E-13,-1.0001463424449E-12));
#27490=DIRECTION('',(-9.99479153109778E-13,-1.,1.00002200371E-12));
#27491=DIRECTION('',(-1.,9.99435799370104E-13,-1.0001463424449E-12));
#27492=DIRECTION('center_axis',(-5.6420062889324E-16,1.,6.61092274672781E-17));
#27493=DIRECTION('ref_axis',(-1.06105803387953E-14,6.61092274672721E-17,
-1.));
#27494=DIRECTION('',(-1.00001914094642E-12,1.00002200370999E-12,1.));
#27495=DIRECTION('',(9.99999999998993E-13,-1.00002200370999E-12,-1.));
#27496=DIRECTION('',(-1.,9.99435799370104E-13,-1.0001463424449E-12));
#27497=DIRECTION('center_axis',(-1.46342445914518E-16,4.46289580949563E-15,
1.));
#27498=DIRECTION('ref_axis',(1.,3.89820370584558E-15,1.46342445914501E-16));
#27499=DIRECTION('',(-9.9948579722165E-13,-1.,1.0044628958085E-12));
#27500=DIRECTION('',(9.99479153109778E-13,1.,-1.0044628958085E-12));
#27501=DIRECTION('',(-1.,9.99435799370104E-13,-1.0001463424449E-12));
#27502=DIRECTION('center_axis',(5.64200628893241E-16,-1.,2.20037109950003E-17));
#27503=DIRECTION('ref_axis',(-1.,-5.64200628893241E-16,1.0522467400333E-14));
#27504=DIRECTION('',(1.00001914094642E-12,-1.00002200370999E-12,-1.));
#27505=DIRECTION('',(-9.99999999998993E-13,1.00002200370999E-12,1.));
#27506=DIRECTION('center_axis',(-5.6420062889325E-16,1.,6.61092274672818E-17));
#27507=DIRECTION('ref_axis',(-9.50035731417012E-15,6.61092274672764E-17,
-1.));
#27508=DIRECTION('',(-1.00001914094641E-12,-1.00108821931263E-12,1.));
#27509=DIRECTION('',(-1.,9.99435799370104E-13,-1.0001463424449E-12));
#27510=DIRECTION('',(9.99999999998985E-13,1.00108821931263E-12,-1.));
#27511=DIRECTION('',(-1.,9.99435799370104E-13,-1.0001463424449E-12));
#27512=DIRECTION('center_axis',(-1.46342445914518E-16,4.46289580949563E-15,
1.));
#27513=DIRECTION('ref_axis',(1.,3.89820370584558E-15,1.46342445914501E-16));
#27514=DIRECTION('',(-9.9948579722165E-13,-1.,1.0044628958085E-12));
#27515=DIRECTION('',(9.99479153109778E-13,1.,-1.0044628958085E-12));
#27516=DIRECTION('',(-1.,9.99435799370104E-13,-1.0001463424449E-12));
#27517=DIRECTION('center_axis',(5.64200628893241E-16,-1.,2.20037109950003E-17));
#27518=DIRECTION('ref_axis',(-1.,-5.64200628893241E-16,1.0522467400333E-14));
#27519=DIRECTION('',(1.00001914094642E-12,-1.00002200370999E-12,-1.));
#27520=DIRECTION('',(-9.99999999998993E-13,1.00002200370999E-12,1.));
#27521=DIRECTION('',(-1.,9.99435799370104E-13,-1.0001463424449E-12));
#27522=DIRECTION('center_axis',(-1.0522467400333E-14,-4.46289580949556E-15,
-1.));
#27523=DIRECTION('ref_axis',(1.,-6.77060614040192E-15,-1.0522467400333E-14));
#27524=DIRECTION('',(9.9948579722165E-13,1.,-1.0044628958085E-12));
#27525=DIRECTION('',(-9.99479153109778E-13,-1.,1.0044628958085E-12));
#27526=DIRECTION('center_axis',(5.64200628893243E-16,-1.,1.13222673562016E-15));
#27527=DIRECTION('ref_axis',(-1.,-5.64200628893231E-16,1.0522467400333E-14));
#27528=DIRECTION('',(1.00001914094642E-12,-1.00113222673461E-12,-1.));
#27529=DIRECTION('',(-1.,9.99435799370104E-13,-1.00027970256798E-12));
#27530=DIRECTION('',(-9.99999999998993E-13,1.00113222673461E-12,1.));
#27531=DIRECTION('',(-1.,9.99435799370104E-13,-1.00027970256798E-12));
#27532=DIRECTION('center_axis',(-1.0522467400333E-14,2.19844233825538E-15,
-1.));
#27533=DIRECTION('ref_axis',(1.,-6.90396626348002E-15,-1.0522467400333E-14));
#27534=DIRECTION('',(9.99485797221669E-13,1.,1.00219844233724E-12));
#27535=DIRECTION('',(-9.99479153109799E-13,-1.,-1.00219844233724E-12));
#27536=DIRECTION('',(-1.,9.99435799370104E-13,-1.00027970256798E-12));
#27537=DIRECTION('center_axis',(-5.6420062889324E-16,1.,6.61092274672781E-17));
#27538=DIRECTION('ref_axis',(-1.06105803387953E-14,6.61092274672721E-17,
-1.));
#27539=DIRECTION('',(-1.00001914094642E-12,1.00002200370999E-12,1.));
#27540=DIRECTION('',(9.99999999998993E-13,-1.00002200370999E-12,-1.));
#27541=DIRECTION('',(-1.,9.99435799370104E-13,-1.00027970256798E-12));
#27542=DIRECTION('center_axis',(-2.79702568992582E-16,-4.41888838750562E-15,
1.));
#27543=DIRECTION('ref_axis',(1.,3.89820370584558E-15,2.79702568992599E-16));
#27544=DIRECTION('',(-9.99485797221669E-13,-1.,-1.00441888838649E-12));
#27545=DIRECTION('',(9.99479153109799E-13,1.,1.00441888838649E-12));
#27546=DIRECTION('center_axis',(5.64200628893241E-16,-1.,2.20037109950003E-17));
#27547=DIRECTION('ref_axis',(-1.,-5.64200628893241E-16,1.0522467400333E-14));
#27548=DIRECTION('',(1.00001914094642E-12,-1.00002200370999E-12,-1.));
#27549=DIRECTION('',(-1.,9.99435799370104E-13,-1.0001463424449E-12));
#27550=DIRECTION('',(-9.99999999998993E-13,1.00002200370999E-12,1.));
#27551=DIRECTION('',(-1.,9.99435799370104E-13,-1.0001463424449E-12));
#27552=DIRECTION('center_axis',(-1.0522467400333E-14,-2.2003710994928E-17,
-1.));
#27553=DIRECTION('ref_axis',(1.,-6.77060614040192E-15,-1.0522467400333E-14));
#27554=DIRECTION('',(9.99485797221648E-13,1.,-1.00002200371E-12));
#27555=DIRECTION('',(-9.99479153109778E-13,-1.,1.00002200371E-12));
#27556=DIRECTION('',(-1.,9.99435799370104E-13,-1.0001463424449E-12));
#27557=DIRECTION('center_axis',(-5.6420062889324E-16,1.,6.61092274672781E-17));
#27558=DIRECTION('ref_axis',(-1.06105803387953E-14,6.61092274672721E-17,
-1.));
#27559=DIRECTION('',(-1.00001914094642E-12,1.00002200370999E-12,1.));
#27560=DIRECTION('',(9.99999999998993E-13,-1.00002200370999E-12,-1.));
#27561=DIRECTION('',(-1.,9.99435799370104E-13,-1.0001463424449E-12));
#27562=DIRECTION('center_axis',(-1.46342445914501E-16,2.20037109950002E-17,
1.));
#27563=DIRECTION('ref_axis',(1.,3.89820370584558E-15,1.46342445914501E-16));
#27564=DIRECTION('',(-9.99485797221648E-13,-1.,1.00002200371E-12));
#27565=DIRECTION('',(9.99479153109778E-13,1.,-1.00002200371E-12));
#27566=DIRECTION('center_axis',(-1.,-3.89820370584558E-15,2.74254865331501E-16));
#27567=DIRECTION('ref_axis',(3.89820370584558E-15,-1.,-6.61092274673135E-17));
#27568=DIRECTION('',(-9.99725745133657E-13,-6.61092274712107E-17,1.));
#27569=DIRECTION('',(-9.96101796293144E-13,-1.,9.99999999999011E-13));
#27570=DIRECTION('',(-9.99725745133657E-13,-6.61092274712107E-17,1.));
#27571=DIRECTION('',(9.96101796293144E-13,1.,-9.99999999999011E-13));
#27572=DIRECTION('center_axis',(-3.89820370584558E-15,1.,6.61092274673135E-17));
#27573=DIRECTION('ref_axis',(-1.0522467400333E-14,6.61092274672725E-17,
-1.));
#27574=DIRECTION('',(-1.,-3.89820370584552E-15,-9.99999999998989E-13));
#27575=DIRECTION('',(9.99999999998989E-13,6.61092274712117E-17,-1.));
#27576=DIRECTION('',(1.,3.89820370584552E-15,9.99999999998989E-13));
#27577=DIRECTION('center_axis',(3.89820370584558E-15,-1.,-6.61092274673135E-17));
#27578=DIRECTION('ref_axis',(-1.,-3.89820370584558E-15,1.0522467400333E-14));
#27579=DIRECTION('',(1.,3.89820370584552E-15,9.99999999998989E-13));
#27580=DIRECTION('',(-1.,-3.89820370584552E-15,-9.99999999998989E-13));
#27581=DIRECTION('',(-9.99999999998989E-13,-6.61092274712117E-17,1.));
#27582=DIRECTION('center_axis',(0.,3.71824206197546E-31,1.));
#27583=DIRECTION('ref_axis',(1.,3.89820370584558E-15,-1.44944649852236E-45));
#27584=DIRECTION('',(-9.60161374617363E-15,-1.,1.E-14));
#27585=DIRECTION('',(1.,-9.60161374617374E-15,9.9999999999998E-15));
#27586=DIRECTION('',(9.47915311079142E-15,1.,-1.E-14));
#27587=DIRECTION('',(1.,-9.99693694313996E-13,9.99999999998989E-13));
#27588=DIRECTION('',(-9.60161374617363E-15,-1.,1.E-14));
#27589=DIRECTION('center_axis',(-1.,-3.98386253826119E-16,0.));
#27590=DIRECTION('ref_axis',(3.98386253826119E-16,-1.,-6.61092274672767E-17));
#27591=DIRECTION('',(-9.60161374617363E-15,-1.,1.E-14));
#27592=DIRECTION('',(9.99999999999984E-15,-9.99999999999985E-15,-1.));
#27593=DIRECTION('',(-9.60670630755441E-15,-1.,1.E-14));
#27594=DIRECTION('',(-9.99999999999984E-15,9.99999999999985E-15,1.));
#27595=DIRECTION('center_axis',(-3.0630568499948E-16,1.,6.61092274672757E-17));
#27596=DIRECTION('ref_axis',(-1.0522467400333E-14,6.61092274672725E-17,
-1.));
#27597=DIRECTION('',(-1.00001914094642E-12,9.99933890771529E-13,1.));
#27598=DIRECTION('',(-1.,9.99693694313996E-13,-9.99999999998989E-13));
#27599=DIRECTION('',(9.99999999998993E-13,-9.99933890771529E-13,-1.));
#27600=DIRECTION('center_axis',(1.,5.1420277733694E-16,-1.0522467400333E-14));
#27601=DIRECTION('ref_axis',(-1.0522467400333E-14,1.06077175752244E-14,
-1.));
#27602=DIRECTION('',(-9.99999999999984E-15,9.99999999999985E-15,1.));
#27603=DIRECTION('',(-9.99485797221669E-13,-1.,-1.0001493759533E-12));
#27604=DIRECTION('',(1.00001914094641E-12,1.00006610922647E-12,-1.));
#27605=DIRECTION('',(9.99485797221669E-13,1.,1.00006610922646E-12));
#27606=DIRECTION('',(-9.99999999999984E-15,9.99999999999985E-15,1.));
#27607=DIRECTION('',(-9.99485797221669E-13,-1.,-1.00006610922646E-12));
#27608=DIRECTION('',(1.00001914094642E-12,-9.99933890771529E-13,-1.));
#27609=DIRECTION('',(9.99485797221669E-13,1.,1.0001493759533E-12));
#27610=DIRECTION('',(-9.99999999999984E-15,9.99999999999985E-15,1.));
#27611=DIRECTION('',(9.47915311079142E-15,1.,-1.E-14));
#27612=DIRECTION('center_axis',(3.36838938541509E-16,-1.,-6.61092274673116E-17));
#27613=DIRECTION('ref_axis',(-1.,-3.3683893854151E-16,1.0522467400333E-14));
#27614=DIRECTION('',(9.99999999999984E-15,-9.99999999999985E-15,-1.));
#27615=DIRECTION('',(-1.,9.99645538472762E-13,-9.99999999998989E-13));
#27616=DIRECTION('',(1.,-9.99663161060454E-13,9.99999999998989E-13));
#27617=DIRECTION('center_axis',(1.,-3.83971434457208E-15,-1.05224674003331E-14));
#27618=DIRECTION('ref_axis',(-1.05224674003331E-14,1.00581164490937E-14,
-1.));
#27619=DIRECTION('',(-1.00383971434355E-12,-1.,9.99999999999011E-13));
#27620=DIRECTION('',(9.99469539820287E-13,-9.99999999998997E-13,-1.));
#27621=DIRECTION('',(1.00383971434355E-12,1.,-9.99999999999011E-13));
#27622=DIRECTION('',(-9.99469539820287E-13,9.99999999998997E-13,1.));
#27623=DIRECTION('center_axis',(5.30460178706591E-16,-6.61092274673115E-17,
1.));
#27624=DIRECTION('ref_axis',(1.,3.89820370584558E-15,-5.30460178706591E-16));
#27625=DIRECTION('',(-1.,9.9960161374517E-13,-9.99469539820283E-13));
#27626=DIRECTION('',(1.,-9.9960670630655E-13,9.99469539820283E-13));
#27627=DIRECTION('center_axis',(-3.9329369244535E-16,1.,6.61092274672764E-17));
#27628=DIRECTION('ref_axis',(-1.05885766278003E-14,6.61092274672722E-17,
-1.));
#27629=DIRECTION('',(1.,-9.60670630755452E-15,9.9999999999998E-15));
#27630=DIRECTION('',(9.99999999999984E-15,-9.99999999999985E-15,-1.));
#27631=DIRECTION('',(1.,-9.60670630755452E-15,1.01020425574102E-14));
#27632=DIRECTION('',(9.99999999999984E-15,-9.99999999999985E-15,-1.));
#27633=DIRECTION('center_axis',(3.98386253826121E-16,-1.,1.20031049926069E-31));
#27634=DIRECTION('ref_axis',(-1.,-3.98386253826121E-16,1.0522467400333E-14));
#27635=DIRECTION('',(1.,-9.9960161374517E-13,9.99999999998989E-13));
#27636=DIRECTION('',(1.,-9.9960161374517E-13,1.00057976284491E-12));
#27637=DIRECTION('',(-1.00057976284491E-12,9.99999999998997E-13,1.));
#27638=DIRECTION('',(-1.,9.9960161374517E-13,-9.99999999998989E-13));
#27639=DIRECTION('',(1.,-9.60161374617374E-15,1.0306127672231E-14));
#27640=DIRECTION('',(-1.01141265444719E-14,9.99999999999985E-15,1.));
#27641=DIRECTION('',(-1.,9.60161374617374E-15,-1.01020425574102E-14));
#27642=DIRECTION('',(-9.99999999999984E-15,9.99999999999985E-15,1.));
#27643=DIRECTION('',(1.,-9.60161374617374E-15,9.9999999999998E-15));
#27644=DIRECTION('center_axis',(4.794216935078E-16,-1.,-6.61092274673155E-17));
#27645=DIRECTION('ref_axis',(-1.,-4.79421693507801E-16,1.0522467400333E-14));
#27646=DIRECTION('',(9.99999999999984E-15,-9.99999999999985E-15,-1.));
#27647=DIRECTION('',(-1.,9.99520578305488E-13,-9.99999999998989E-13));
#27648=DIRECTION('',(-1.,9.99520578305488E-13,-9.99999999998989E-13));
#27649=DIRECTION('center_axis',(1.,-2.9746054942148E-15,-1.05224674003331E-14));
#27650=DIRECTION('ref_axis',(-1.05224674003331E-14,1.11683394737189E-14,
-1.));
#27651=DIRECTION('',(-1.0029746054932E-12,-1.,9.99999999999011E-13));
#27652=DIRECTION('',(-1.0029746054932E-12,-1.,9.99999999999011E-13));
#27653=DIRECTION('',(1.00057976284491E-12,-9.99999999998997E-13,-1.));
#27654=DIRECTION('center_axis',(-1.0522467400333E-14,6.61092274673958E-17,
-1.));
#27655=DIRECTION('ref_axis',(1.,-7.20402654040602E-15,-1.0522467400333E-14));
#27656=DIRECTION('',(-1.,9.9960670630655E-13,-1.00057976284491E-12));
#27657=DIRECTION('center_axis',(-1.,-3.89820370584558E-15,2.74254865331601E-16));
#27658=DIRECTION('ref_axis',(3.89820370584558E-15,-1.,-6.61092274673135E-17));
#27659=DIRECTION('',(-9.99725745133657E-13,-6.61092274712107E-17,1.));
#27660=DIRECTION('',(9.96101796293144E-13,1.,-9.99999999999011E-13));
#27661=DIRECTION('',(9.99725745133657E-13,6.61092274712107E-17,-1.));
#27662=DIRECTION('',(-9.96101796293144E-13,-1.,9.99999999999011E-13));
#27663=DIRECTION('center_axis',(3.89820370584558E-15,-1.,-6.61092274673135E-17));
#27664=DIRECTION('ref_axis',(-1.,-3.89820370584558E-15,1.0522467400333E-14));
#27665=DIRECTION('',(-1.,-3.89820370584552E-15,-9.99999999998989E-13));
#27666=DIRECTION('',(9.99999999998989E-13,6.61092274712117E-17,-1.));
#27667=DIRECTION('',(1.,3.89820370584552E-15,9.99999999998989E-13));
#27668=DIRECTION('center_axis',(3.89820370584558E-15,-1.,-6.61092274673135E-17));
#27669=DIRECTION('ref_axis',(-1.,-3.89820370584558E-15,1.0522467400333E-14));
#27670=DIRECTION('',(1.,3.89820370584552E-15,9.99999999998989E-13));
#27671=DIRECTION('',(-1.,-3.89820370584552E-15,-9.99999999998989E-13));
#27672=DIRECTION('',(-9.99999999998989E-13,-6.61092274712117E-17,1.));
#27673=DIRECTION('center_axis',(-1.,-3.98386253826119E-16,0.));
#27674=DIRECTION('ref_axis',(3.98386253826119E-16,-1.,-6.61092274672767E-17));
#27675=DIRECTION('',(-9.60161374617363E-15,-1.,1.E-14));
#27676=DIRECTION('',(-9.60161374617363E-15,-1.,1.E-14));
#27677=DIRECTION('',(9.99999999999984E-15,-9.99999999999985E-15,-1.));
#27678=DIRECTION('',(-9.60161374617363E-15,-1.,1.E-14));
#27679=DIRECTION('center_axis',(-1.,-3.98386253826119E-16,0.));
#27680=DIRECTION('ref_axis',(3.98386253826119E-16,-1.,-6.61092274672767E-17));
#27681=DIRECTION('',(-9.60161374617363E-15,-1.,1.E-14));
#27682=DIRECTION('',(-9.60670630755441E-15,-1.,1.E-14));
#27683=DIRECTION('',(-9.60161374617363E-15,-1.,1.E-14));
#27684=DIRECTION('center_axis',(0.,3.71824206197546E-31,1.));
#27685=DIRECTION('ref_axis',(1.,3.89820370584558E-15,-1.44944649852236E-45));
#27686=DIRECTION('center_axis',(-1.0522467400333E-14,7.23040323441634E-29,
-1.));
#27687=DIRECTION('ref_axis',(1.,-6.72630625189782E-15,-1.0522467400333E-14));
#27688=DIRECTION('',(-9.60670630755441E-15,-1.,1.E-14));
#27689=DIRECTION('center_axis',(0.,3.71824206197546E-31,1.));
#27690=DIRECTION('ref_axis',(1.,3.89820370584558E-15,-1.44944649852236E-45));
#27691=DIRECTION('',(9.47915311079142E-15,1.,-1.E-14));
#27692=DIRECTION('',(0.707106781186548,0.707106781186547,9.99999999999976E-15));
#27693=DIRECTION('',(9.47915311079142E-15,1.,-1.E-14));
#27694=DIRECTION('',(-1.,9.65799058254168E-15,-9.9999999999998E-15));
#27695=DIRECTION('center_axis',(3.42009417458172E-16,-1.,7.1325447274173E-31));
#27696=DIRECTION('ref_axis',(-1.,-3.42009417458172E-16,1.0522467400333E-14));
#27697=DIRECTION('',(9.99999999999984E-15,-9.99999999999985E-15,-1.));
#27698=DIRECTION('',(-1.,9.65799058254168E-15,-9.9999999999998E-15));
#27699=DIRECTION('center_axis',(0.,3.71824206197546E-31,1.));
#27700=DIRECTION('ref_axis',(1.,3.89820370584558E-15,-1.44944649852236E-45));
#27701=DIRECTION('',(9.47915311079142E-15,1.,-1.E-14));
#27702=DIRECTION('',(0.707106781186548,0.707106781186547,9.99999999999976E-15));
#27703=DIRECTION('',(9.47915311079142E-15,1.,-1.E-14));
#27704=DIRECTION('',(1.,-9.60670630755452E-15,9.9999999999998E-15));
#27705=DIRECTION('center_axis',(-3.9329369244535E-16,1.,6.61092274672764E-17));
#27706=DIRECTION('ref_axis',(-1.05885766278003E-14,6.61092274672722E-17,
-1.));
#27707=DIRECTION('',(9.99999999999984E-15,-9.99999999999985E-15,-1.));
#27708=DIRECTION('',(-1.,9.60670630755452E-15,-1.0306127672231E-14));
#27709=DIRECTION('center_axis',(-3.06127672231199E-16,-2.03369632909008E-32,
1.));
#27710=DIRECTION('ref_axis',(1.,3.89820370584558E-15,3.06127672231199E-16));
#27711=DIRECTION('',(-9.60670630755441E-15,-1.,1.E-14));
#27712=DIRECTION('center_axis',(-1.,-5.20846889208359E-16,0.));
#27713=DIRECTION('ref_axis',(5.20846889208359E-16,-1.,-6.6109227467278E-17));
#27714=DIRECTION('',(9.99999999999984E-15,-9.99999999999985E-15,-1.));
#27715=DIRECTION('center_axis',(-0.707106781186547,0.707106781186548,1.10440526730942E-29));
#27716=DIRECTION('ref_axis',(-6.61092274672986E-17,-6.61092274673141E-17,
1.));
#27717=DIRECTION('',(9.99999999999984E-15,-9.99999999999985E-15,-1.));
#27718=DIRECTION('center_axis',(-1.,-5.20846889208359E-16,0.));
#27719=DIRECTION('ref_axis',(5.20846889208359E-16,-1.,-6.6109227467278E-17));
#27720=DIRECTION('axis',(0.,0.,1.));
#27721=DIRECTION('refdir',(1.,0.,0.));
#27722=DIRECTION('center_axis',(-6.65798752924967E-17,1.,-1.71022579061586E-31));
#27723=DIRECTION('ref_axis',(0.211873077029416,1.41064830464559E-17,-0.97729719084324));
#27724=DIRECTION('center_axis',(6.65798752924967E-17,-1.,1.71022579061586E-31));
#27725=DIRECTION('ref_axis',(0.211873077029416,1.41064830464559E-17,-0.977297190843239));
#27726=DIRECTION('',(-6.65798752924967E-17,1.,-1.71022579061586E-31));
#27727=DIRECTION('center_axis',(-6.65798752924967E-17,1.,-1.71022579061586E-31));
#27728=DIRECTION('ref_axis',(0.211873077029416,1.41064830464559E-17,-0.977297190843239));
#27729=DIRECTION('center_axis',(-6.65798752924967E-17,1.,-1.71022579061586E-31));
#27730=DIRECTION('ref_axis',(-0.211873077029416,-1.41064830464559E-17,0.977297190843239));
#27731=DIRECTION('center_axis',(6.65798752924967E-17,-1.,1.71022579061586E-31));
#27732=DIRECTION('ref_axis',(-0.211873077029416,-1.41064830464559E-17,0.977297190843239));
#27733=DIRECTION('',(6.65798752924967E-17,-1.,1.71022579061586E-31));
#27734=DIRECTION('center_axis',(-6.65798752924967E-17,1.,-1.71022579061586E-31));
#27735=DIRECTION('ref_axis',(-0.211873077029416,-1.41064830464559E-17,0.977297190843239));
#27736=DIRECTION('center_axis',(-6.65798752924967E-17,1.,-1.71022579061586E-31));
#27737=DIRECTION('ref_axis',(-0.211873077029416,-1.41064830464559E-17,0.97729719084324));
#27738=DIRECTION('center_axis',(-6.65798752924967E-17,1.,-1.71022579061586E-31));
#27739=DIRECTION('ref_axis',(-0.211873077029416,-1.41064830464559E-17,0.97729719084324));
#27740=DIRECTION('axis',(0.,0.,1.));
#27741=DIRECTION('refdir',(1.,0.,0.));
#27742=DIRECTION('center_axis',(0.,-1.,0.));
#27743=DIRECTION('ref_axis',(-0.281918008728671,0.,0.95943850055877));
#27744=DIRECTION('center_axis',(0.,1.,0.));
#27745=DIRECTION('ref_axis',(-0.281918008754672,0.,0.95943850055113));
#27746=DIRECTION('',(0.,-1.,0.));
#27747=DIRECTION('center_axis',(0.,-1.,0.));
#27748=DIRECTION('ref_axis',(-0.281918008754672,0.,0.95943850055113));
#27749=DIRECTION('',(0.,1.,0.));
#27750=DIRECTION('center_axis',(0.,-1.,0.));
#27751=DIRECTION('ref_axis',(0.470745247127108,0.,0.882269183586981));
#27752=DIRECTION('center_axis',(0.,-1.,0.));
#27753=DIRECTION('ref_axis',(0.470745247127378,0.,0.882269183586837));
#27754=DIRECTION('',(0.,1.,0.));
#27755=DIRECTION('center_axis',(0.,1.,0.));
#27756=DIRECTION('ref_axis',(0.470745247127378,0.,0.882269183586837));
#27757=DIRECTION('center_axis',(0.,-1.,0.));
#27758=DIRECTION('ref_axis',(0.971857119217081,0.,0.235571092936032));
#27759=DIRECTION('center_axis',(0.,1.,0.));
#27760=DIRECTION('ref_axis',(0.971857119210143,0.,0.235571092964655));
#27761=DIRECTION('',(0.,-1.,0.));
#27762=DIRECTION('center_axis',(0.,-1.,0.));
#27763=DIRECTION('ref_axis',(0.971857119210143,0.,0.235571092964655));
#27764=DIRECTION('center_axis',(0.848811934516349,0.,-0.528694902398929));
#27765=DIRECTION('ref_axis',(0.,-1.,0.));
#27766=DIRECTION('',(0.528694902399201,0.,0.84881193451618));
#27767=DIRECTION('',(0.,1.,0.));
#27768=DIRECTION('',(-0.528694902399201,0.,-0.84881193451618));
#27769=DIRECTION('center_axis',(0.,-1.,0.));
#27770=DIRECTION('ref_axis',(-0.154274306935522,0.,0.9880280553808));
#27771=DIRECTION('center_axis',(0.,1.,0.));
#27772=DIRECTION('ref_axis',(-0.154274306968473,0.,0.988028055375654));
#27773=DIRECTION('',(0.,-1.,0.));
#27774=DIRECTION('center_axis',(0.,-1.,0.));
#27775=DIRECTION('ref_axis',(-0.154274306968473,0.,0.988028055375654));
#27776=DIRECTION('',(0.,1.,0.));
#27777=DIRECTION('center_axis',(0.,-1.,0.));
#27778=DIRECTION('ref_axis',(0.581877193327017,0.,0.813276663802591));
#27779=DIRECTION('center_axis',(0.,-1.,0.));
#27780=DIRECTION('ref_axis',(0.581877193327157,0.,0.813276663802491));
#27781=DIRECTION('',(0.,1.,0.));
#27782=DIRECTION('center_axis',(0.,1.,0.));
#27783=DIRECTION('ref_axis',(0.581877193327157,0.,0.813276663802491));
#27784=DIRECTION('center_axis',(0.,-1.,0.));
#27785=DIRECTION('ref_axis',(0.994290944595386,0.,0.106702940426287));
#27786=DIRECTION('center_axis',(0.,1.,0.));
#27787=DIRECTION('ref_axis',(0.994290944591597,0.,0.106702940461588));
#27788=DIRECTION('',(0.,-1.,0.));
#27789=DIRECTION('center_axis',(0.,-1.,0.));
#27790=DIRECTION('ref_axis',(0.994290944591597,0.,0.106702940461588));
#27791=DIRECTION('center_axis',(0.772541698292714,0.,-0.634964033941301));
#27792=DIRECTION('ref_axis',(0.,-1.,0.));
#27793=DIRECTION('',(0.634964033941407,0.,0.772541698292626));
#27794=DIRECTION('',(0.,1.,0.));
#27795=DIRECTION('',(-0.634964033941407,0.,-0.772541698292626));
#27796=DIRECTION('center_axis',(0.,-1.,0.));
#27797=DIRECTION('ref_axis',(-0.0239909289777986,0.,0.999712176242133));
#27798=DIRECTION('center_axis',(0.,1.,0.));
#27799=DIRECTION('ref_axis',(-0.0239909290168162,0.,0.999712176241197));
#27800=DIRECTION('',(0.,-1.,0.));
#27801=DIRECTION('center_axis',(0.,-1.,0.));
#27802=DIRECTION('ref_axis',(-0.0239909290168162,0.,0.999712176241197));
#27803=DIRECTION('',(0.,1.,0.));
#27804=DIRECTION('center_axis',(0.,-1.,0.));
#27805=DIRECTION('ref_axis',(0.683053059422266,0.,0.730368754817649));
#27806=DIRECTION('center_axis',(0.,-1.,0.));
#27807=DIRECTION('ref_axis',(0.683053059422291,0.,0.730368754817625));
#27808=DIRECTION('',(0.,1.,0.));
#27809=DIRECTION('center_axis',(0.,1.,0.));
#27810=DIRECTION('ref_axis',(0.683053059422291,0.,0.730368754817625));
#27811=DIRECTION('center_axis',(0.,-1.,0.));
#27812=DIRECTION('ref_axis',(0.999712176242133,0.,-0.0239909289777986));
#27813=DIRECTION('center_axis',(0.,1.,0.));
#27814=DIRECTION('ref_axis',(0.999712176241197,0.,-0.0239909290168162));
#27815=DIRECTION('',(0.,-1.,0.));
#27816=DIRECTION('center_axis',(0.,-1.,0.));
#27817=DIRECTION('ref_axis',(0.999712176241197,0.,-0.0239909290168162));
#27818=DIRECTION('center_axis',(0.683053059422266,0.,-0.730368754817649));
#27819=DIRECTION('ref_axis',(0.,-1.,0.));
#27820=DIRECTION('',(0.730368754817616,0.,0.683053059422301));
#27821=DIRECTION('',(0.,1.,0.));
#27822=DIRECTION('',(-0.730368754817616,0.,-0.683053059422301));
#27823=DIRECTION('center_axis',(0.,-1.,0.));
#27824=DIRECTION('ref_axis',(0.106702940426287,0.,0.994290944595386));
#27825=DIRECTION('center_axis',(0.,1.,0.));
#27826=DIRECTION('ref_axis',(0.106702940461588,0.,0.994290944591597));
#27827=DIRECTION('',(0.,-1.,0.));
#27828=DIRECTION('center_axis',(0.,-1.,0.));
#27829=DIRECTION('ref_axis',(0.106702940461588,0.,0.994290944591597));
#27830=DIRECTION('',(0.,1.,0.));
#27831=DIRECTION('center_axis',(0.,-1.,0.));
#27832=DIRECTION('ref_axis',(0.772541698292714,0.,0.634964033941301));
#27833=DIRECTION('center_axis',(0.,-1.,0.));
#27834=DIRECTION('ref_axis',(0.772541698292649,0.,0.63496403394138));
#27835=DIRECTION('',(0.,1.,0.));
#27836=DIRECTION('center_axis',(0.,1.,0.));
#27837=DIRECTION('ref_axis',(0.772541698292649,0.,0.63496403394138));
#27838=DIRECTION('center_axis',(0.,-1.,0.));
#27839=DIRECTION('ref_axis',(0.988028055380798,0.,-0.15427430693553));
#27840=DIRECTION('center_axis',(0.,1.,0.));
#27841=DIRECTION('ref_axis',(0.988028055375653,0.,-0.154274306968481));
#27842=DIRECTION('',(0.,-1.,0.));
#27843=DIRECTION('center_axis',(0.,-1.,0.));
#27844=DIRECTION('ref_axis',(0.988028055375653,0.,-0.154274306968481));
#27845=DIRECTION('center_axis',(0.581877193327018,0.,-0.813276663802591));
#27846=DIRECTION('ref_axis',(0.,-1.,0.));
#27847=DIRECTION('',(0.813276663802457,0.,0.581877193327205));
#27848=DIRECTION('',(0.,1.,0.));
#27849=DIRECTION('',(-0.813276663802457,0.,-0.581877193327205));
#27850=DIRECTION('center_axis',(0.,-1.,0.));
#27851=DIRECTION('ref_axis',(0.235571092936033,0.,0.971857119217081));
#27852=DIRECTION('center_axis',(0.,1.,0.));
#27853=DIRECTION('ref_axis',(0.235571092964656,0.,0.971857119210143));
#27854=DIRECTION('',(0.,-1.,0.));
#27855=DIRECTION('center_axis',(0.,-1.,0.));
#27856=DIRECTION('ref_axis',(0.235571092964656,0.,0.971857119210143));
#27857=DIRECTION('',(0.,1.,0.));
#27858=DIRECTION('center_axis',(0.,-1.,0.));
#27859=DIRECTION('ref_axis',(0.848811934516349,0.,0.528694902398929));
#27860=DIRECTION('center_axis',(0.,-1.,0.));
#27861=DIRECTION('ref_axis',(0.848811934516223,0.,0.528694902399131));
#27862=DIRECTION('',(0.,1.,0.));
#27863=DIRECTION('center_axis',(0.,1.,0.));
#27864=DIRECTION('ref_axis',(0.848811934516223,0.,0.528694902399131));
#27865=DIRECTION('center_axis',(0.,-1.,0.));
#27866=DIRECTION('ref_axis',(0.959438500558773,0.,-0.28191800872866));
#27867=DIRECTION('center_axis',(0.,1.,0.));
#27868=DIRECTION('ref_axis',(0.959438500551133,0.,-0.281918008754661));
#27869=DIRECTION('',(0.,-1.,0.));
#27870=DIRECTION('center_axis',(0.,-1.,0.));
#27871=DIRECTION('ref_axis',(0.959438500551133,0.,-0.281918008754661));
#27872=DIRECTION('center_axis',(0.470745247127108,0.,-0.882269183586981));
#27873=DIRECTION('ref_axis',(0.,-1.,0.));
#27874=DIRECTION('',(0.882269183586787,0.,0.470745247127471));
#27875=DIRECTION('',(0.,1.,0.));
#27876=DIRECTION('',(-0.882269183586787,0.,-0.470745247127471));
#27877=DIRECTION('center_axis',(-0.528694902398929,0.,0.848811934516349));
#27878=DIRECTION('ref_axis',(0.,1.,0.));
#27879=DIRECTION('',(0.84881193451618,0.,0.528694902399201));
#27880=DIRECTION('',(0.,-1.,0.));
#27881=DIRECTION('',(-0.84881193451618,0.,-0.528694902399201));
#27882=DIRECTION('center_axis',(-0.634964033941301,0.,0.772541698292714));
#27883=DIRECTION('ref_axis',(0.,1.,0.));
#27884=DIRECTION('',(0.772541698292626,0.,0.634964033941407));
#27885=DIRECTION('',(0.,-1.,0.));
#27886=DIRECTION('',(-0.772541698292626,0.,-0.634964033941407));
#27887=DIRECTION('center_axis',(-0.813276663802591,0.,0.581877193327018));
#27888=DIRECTION('ref_axis',(0.,1.,0.));
#27889=DIRECTION('',(0.581877193327206,0.,0.813276663802456));
#27890=DIRECTION('',(0.,-1.,0.));
#27891=DIRECTION('',(-0.581877193327206,0.,-0.813276663802456));
#27892=DIRECTION('center_axis',(-0.882269183586981,0.,0.470745247127108));
#27893=DIRECTION('ref_axis',(0.,1.,0.));
#27894=DIRECTION('',(0.470745247127471,0.,0.882269183586787));
#27895=DIRECTION('',(0.,-1.,0.));
#27896=DIRECTION('',(-0.470745247127471,0.,-0.882269183586787));
#27897=DIRECTION('center_axis',(0.,1.,0.));
#27898=DIRECTION('ref_axis',(-0.430511096808295,0.,-0.902585284349861));
#27899=DIRECTION('center_axis',(0.,-1.,0.));
#27900=DIRECTION('ref_axis',(-0.430511096808622,0.,-0.902585284349705));
#27901=DIRECTION('',(0.,-1.,0.));
#27902=DIRECTION('center_axis',(0.,1.,0.));
#27903=DIRECTION('ref_axis',(-0.430511096808622,0.,-0.902585284349705));
#27904=DIRECTION('center_axis',(0.,1.,0.));
#27905=DIRECTION('ref_axis',(-0.430511096808295,0.,-0.902585284349861));
#27906=DIRECTION('center_axis',(0.,1.,0.));
#27907=DIRECTION('ref_axis',(-0.430511096808622,0.,-0.902585284349705));
#27908=DIRECTION('center_axis',(0.,-1.,0.));
#27909=DIRECTION('ref_axis',(-0.430511096808622,0.,-0.902585284349705));
#27910=DIRECTION('center_axis',(0.,1.,0.));
#27911=DIRECTION('ref_axis',(1.,0.,0.));
#27912=DIRECTION('',(0.902585284349658,0.,0.430511096808719));
#27913=DIRECTION('center_axis',(0.,-1.,0.));
#27914=DIRECTION('ref_axis',(0.430511096808602,0.,0.902585284349714));
#27915=DIRECTION('',(-0.430511096808721,0.,-0.902585284349657));
#27916=DIRECTION('center_axis',(0.,1.,0.));
#27917=DIRECTION('ref_axis',(-0.430511096808622,0.,-0.902585284349705));
#27918=DIRECTION('center_axis',(0.,1.,0.));
#27919=DIRECTION('ref_axis',(-0.430511096808622,0.,-0.902585284349705));
#27920=DIRECTION('center_axis',(0.,1.,0.));
#27921=DIRECTION('ref_axis',(-0.430511096808622,0.,-0.902585284349705));
#27922=DIRECTION('',(0.683053059422301,0.,0.730368754817616));
#27923=DIRECTION('center_axis',(0.,1.,0.));
#27924=DIRECTION('ref_axis',(-0.430511096808622,0.,-0.902585284349705));
#27925=DIRECTION('center_axis',(0.,1.,0.));
#27926=DIRECTION('ref_axis',(-0.430511096808295,0.,-0.902585284349861));
#27927=DIRECTION('center_axis',(0.,-1.,0.));
#27928=DIRECTION('ref_axis',(-0.430511096808622,0.,-0.902585284349705));
#27929=DIRECTION('',(0.,-1.,0.));
#27930=DIRECTION('center_axis',(0.,1.,0.));
#27931=DIRECTION('ref_axis',(-0.430511096808295,0.,-0.902585284349861));
#27932=DIRECTION('',(0.,1.,0.));
#27933=DIRECTION('center_axis',(0.,-1.,0.));
#27934=DIRECTION('ref_axis',(-0.430511096808622,0.,-0.902585284349705));
#27935=DIRECTION('center_axis',(-0.730368754817649,0.,0.683053059422266));
#27936=DIRECTION('ref_axis',(0.,1.,0.));
#27937=DIRECTION('',(-0.683053059422301,0.,-0.730368754817616));
#27938=DIRECTION('center_axis',(0.,1.,0.));
#27939=DIRECTION('ref_axis',(-0.430511096808295,0.,-0.902585284349861));
#27940=DIRECTION('center_axis',(0.,-1.,0.));
#27941=DIRECTION('ref_axis',(-0.430511096808622,0.,-0.902585284349705));
#27942=DIRECTION('center_axis',(0.430511096808293,0.,-0.902585284349862));
#27943=DIRECTION('ref_axis',(0.,-1.,0.));
#27944=DIRECTION('',(-0.902585284349658,0.,-0.430511096808719));
#27945=DIRECTION('',(0.,1.,0.));
#27946=DIRECTION('center_axis',(0.,1.,0.));
#27947=DIRECTION('ref_axis',(0.430511096808295,0.,0.902585284349861));
#27948=DIRECTION('center_axis',(0.,1.,0.));
#27949=DIRECTION('ref_axis',(0.430511096808602,0.,0.902585284349714));
#27950=DIRECTION('',(0.,1.,0.));
#27951=DIRECTION('center_axis',(-0.902585284349861,0.,0.430511096808295));
#27952=DIRECTION('ref_axis',(0.,1.,0.));
#27953=DIRECTION('',(0.430511096808721,0.,0.902585284349657));
#27954=DIRECTION('center_axis',(0.,1.,0.));
#27955=DIRECTION('ref_axis',(-0.430511096808295,0.,-0.902585284349861));
#27956=DIRECTION('center_axis',(0.,-1.,0.));
#27957=DIRECTION('ref_axis',(-0.430511096808622,0.,-0.902585284349705));
#27958=DIRECTION('center_axis',(0.,1.,0.));
#27959=DIRECTION('ref_axis',(1.,0.,0.));
#27960=DIRECTION('axis',(0.,0.,1.));
#27961=DIRECTION('refdir',(1.,0.,0.));
#27962=DIRECTION('center_axis',(0.,-1.,0.));
#27963=DIRECTION('ref_axis',(-0.95943850055877,0.,-0.281918008728671));
#27964=DIRECTION('center_axis',(0.,1.,0.));
#27965=DIRECTION('ref_axis',(-0.95943850055113,0.,-0.281918008754672));
#27966=DIRECTION('',(0.,-1.,0.));
#27967=DIRECTION('center_axis',(0.,-1.,0.));
#27968=DIRECTION('ref_axis',(-0.95943850055113,0.,-0.281918008754672));
#27969=DIRECTION('',(0.,1.,0.));
#27970=DIRECTION('center_axis',(0.,-1.,0.));
#27971=DIRECTION('ref_axis',(-0.882269183586981,0.,0.470745247127108));
#27972=DIRECTION('center_axis',(0.,-1.,0.));
#27973=DIRECTION('ref_axis',(-0.882269183586837,0.,0.470745247127378));
#27974=DIRECTION('',(0.,1.,0.));
#27975=DIRECTION('center_axis',(0.,1.,0.));
#27976=DIRECTION('ref_axis',(-0.882269183586837,0.,0.470745247127378));
#27977=DIRECTION('center_axis',(0.,-1.,0.));
#27978=DIRECTION('ref_axis',(-0.235571092936032,0.,0.971857119217081));
#27979=DIRECTION('center_axis',(0.,1.,0.));
#27980=DIRECTION('ref_axis',(-0.235571092964655,0.,0.971857119210143));
#27981=DIRECTION('',(0.,-1.,0.));
#27982=DIRECTION('center_axis',(0.,-1.,0.));
#27983=DIRECTION('ref_axis',(-0.235571092964655,0.,0.971857119210143));
#27984=DIRECTION('center_axis',(0.528694902398929,0.,0.848811934516349));
#27985=DIRECTION('ref_axis',(0.,-1.,0.));
#27986=DIRECTION('',(-0.84881193451618,0.,0.528694902399201));
#27987=DIRECTION('',(0.,1.,0.));
#27988=DIRECTION('',(0.84881193451618,0.,-0.528694902399201));
#27989=DIRECTION('center_axis',(0.,-1.,0.));
#27990=DIRECTION('ref_axis',(-0.9880280553808,0.,-0.154274306935522));
#27991=DIRECTION('center_axis',(0.,1.,0.));
#27992=DIRECTION('ref_axis',(-0.988028055375654,0.,-0.154274306968473));
#27993=DIRECTION('',(0.,-1.,0.));
#27994=DIRECTION('center_axis',(0.,-1.,0.));
#27995=DIRECTION('ref_axis',(-0.988028055375654,0.,-0.154274306968473));
#27996=DIRECTION('',(0.,1.,0.));
#27997=DIRECTION('center_axis',(0.,-1.,0.));
#27998=DIRECTION('ref_axis',(-0.813276663802591,0.,0.581877193327017));
#27999=DIRECTION('center_axis',(0.,-1.,0.));
#28000=DIRECTION('ref_axis',(-0.813276663802491,0.,0.581877193327157));
#28001=DIRECTION('',(0.,1.,0.));
#28002=DIRECTION('center_axis',(0.,1.,0.));
#28003=DIRECTION('ref_axis',(-0.813276663802491,0.,0.581877193327157));
#28004=DIRECTION('center_axis',(0.,-1.,0.));
#28005=DIRECTION('ref_axis',(-0.106702940426287,0.,0.994290944595386));
#28006=DIRECTION('center_axis',(0.,1.,0.));
#28007=DIRECTION('ref_axis',(-0.106702940461588,0.,0.994290944591597));
#28008=DIRECTION('',(0.,-1.,0.));
#28009=DIRECTION('center_axis',(0.,-1.,0.));
#28010=DIRECTION('ref_axis',(-0.106702940461588,0.,0.994290944591597));
#28011=DIRECTION('center_axis',(0.634964033941301,0.,0.772541698292714));
#28012=DIRECTION('ref_axis',(0.,-1.,0.));
#28013=DIRECTION('',(-0.772541698292626,0.,0.634964033941407));
#28014=DIRECTION('',(0.,1.,0.));
#28015=DIRECTION('',(0.772541698292626,0.,-0.634964033941407));
#28016=DIRECTION('center_axis',(0.,-1.,0.));
#28017=DIRECTION('ref_axis',(-0.999712176242133,0.,-0.0239909289777924));
#28018=DIRECTION('center_axis',(0.,1.,0.));
#28019=DIRECTION('ref_axis',(-0.999712176241197,0.,-0.0239909290168101));
#28020=DIRECTION('',(0.,-1.,0.));
#28021=DIRECTION('center_axis',(0.,-1.,0.));
#28022=DIRECTION('ref_axis',(-0.999712176241197,0.,-0.0239909290168101));
#28023=DIRECTION('',(0.,1.,0.));
#28024=DIRECTION('center_axis',(0.,-1.,0.));
#28025=DIRECTION('ref_axis',(-0.730368754817649,0.,0.683053059422266));
#28026=DIRECTION('center_axis',(0.,-1.,0.));
#28027=DIRECTION('ref_axis',(-0.730368754817625,0.,0.683053059422291));
#28028=DIRECTION('',(0.,1.,0.));
#28029=DIRECTION('center_axis',(0.,1.,0.));
#28030=DIRECTION('ref_axis',(-0.730368754817625,0.,0.683053059422291));
#28031=DIRECTION('center_axis',(0.,-1.,0.));
#28032=DIRECTION('ref_axis',(0.0239909289777986,0.,0.999712176242133));
#28033=DIRECTION('center_axis',(0.,1.,0.));
#28034=DIRECTION('ref_axis',(0.0239909290168162,0.,0.999712176241197));
#28035=DIRECTION('',(0.,-1.,0.));
#28036=DIRECTION('center_axis',(0.,-1.,0.));
#28037=DIRECTION('ref_axis',(0.0239909290168162,0.,0.999712176241197));
#28038=DIRECTION('center_axis',(0.730368754817649,0.,0.683053059422266));
#28039=DIRECTION('ref_axis',(0.,-1.,0.));
#28040=DIRECTION('',(-0.683053059422301,0.,0.730368754817616));
#28041=DIRECTION('',(0.,1.,0.));
#28042=DIRECTION('',(0.683053059422301,0.,-0.730368754817616));
#28043=DIRECTION('center_axis',(0.,-1.,0.));
#28044=DIRECTION('ref_axis',(-0.994290944595386,0.,0.106702940426287));
#28045=DIRECTION('center_axis',(0.,1.,0.));
#28046=DIRECTION('ref_axis',(-0.994290944591597,0.,0.106702940461588));
#28047=DIRECTION('',(0.,-1.,0.));
#28048=DIRECTION('center_axis',(0.,-1.,0.));
#28049=DIRECTION('ref_axis',(-0.994290944591597,0.,0.106702940461588));
#28050=DIRECTION('',(0.,1.,0.));
#28051=DIRECTION('center_axis',(0.,-1.,0.));
#28052=DIRECTION('ref_axis',(-0.634964033941301,0.,0.772541698292714));
#28053=DIRECTION('center_axis',(0.,-1.,0.));
#28054=DIRECTION('ref_axis',(-0.63496403394138,0.,0.772541698292649));
#28055=DIRECTION('',(0.,1.,0.));
#28056=DIRECTION('center_axis',(0.,1.,0.));
#28057=DIRECTION('ref_axis',(-0.63496403394138,0.,0.772541698292649));
#28058=DIRECTION('center_axis',(0.,-1.,0.));
#28059=DIRECTION('ref_axis',(0.15427430693553,0.,0.988028055380798));
#28060=DIRECTION('center_axis',(0.,1.,0.));
#28061=DIRECTION('ref_axis',(0.154274306968481,0.,0.988028055375653));
#28062=DIRECTION('',(0.,-1.,0.));
#28063=DIRECTION('center_axis',(0.,-1.,0.));
#28064=DIRECTION('ref_axis',(0.154274306968481,0.,0.988028055375653));
#28065=DIRECTION('center_axis',(0.813276663802591,0.,0.581877193327018));
#28066=DIRECTION('ref_axis',(0.,-1.,0.));
#28067=DIRECTION('',(-0.581877193327205,0.,0.813276663802457));
#28068=DIRECTION('',(0.,1.,0.));
#28069=DIRECTION('',(0.581877193327205,0.,-0.813276663802457));
#28070=DIRECTION('center_axis',(0.,-1.,0.));
#28071=DIRECTION('ref_axis',(-0.971857119217081,0.,0.235571092936033));
#28072=DIRECTION('center_axis',(0.,1.,0.));
#28073=DIRECTION('ref_axis',(-0.971857119210143,0.,0.235571092964656));
#28074=DIRECTION('',(0.,-1.,0.));
#28075=DIRECTION('center_axis',(0.,-1.,0.));
#28076=DIRECTION('ref_axis',(-0.971857119210143,0.,0.235571092964656));
#28077=DIRECTION('',(0.,1.,0.));
#28078=DIRECTION('center_axis',(0.,-1.,0.));
#28079=DIRECTION('ref_axis',(-0.528694902398929,0.,0.848811934516349));
#28080=DIRECTION('center_axis',(0.,-1.,0.));
#28081=DIRECTION('ref_axis',(-0.528694902399131,0.,0.848811934516223));
#28082=DIRECTION('',(0.,1.,0.));
#28083=DIRECTION('center_axis',(0.,1.,0.));
#28084=DIRECTION('ref_axis',(-0.528694902399131,0.,0.848811934516223));
#28085=DIRECTION('center_axis',(0.,-1.,0.));
#28086=DIRECTION('ref_axis',(0.281918008728669,0.,0.959438500558771));
#28087=DIRECTION('center_axis',(0.,1.,0.));
#28088=DIRECTION('ref_axis',(0.28191800875467,0.,0.959438500551131));
#28089=DIRECTION('',(0.,-1.,0.));
#28090=DIRECTION('center_axis',(0.,-1.,0.));
#28091=DIRECTION('ref_axis',(0.28191800875467,0.,0.959438500551131));
#28092=DIRECTION('center_axis',(0.882269183586981,0.,0.470745247127108));
#28093=DIRECTION('ref_axis',(0.,-1.,0.));
#28094=DIRECTION('',(-0.470745247127471,0.,0.882269183586787));
#28095=DIRECTION('',(0.,1.,0.));
#28096=DIRECTION('',(0.470745247127471,0.,-0.882269183586787));
#28097=DIRECTION('center_axis',(-0.848811934516349,0.,-0.528694902398929));
#28098=DIRECTION('ref_axis',(-0.528694902398929,0.,0.848811934516349));
#28099=DIRECTION('',(-0.528694902399201,0.,0.84881193451618));
#28100=DIRECTION('',(0.,-1.,0.));
#28101=DIRECTION('',(0.528694902399201,0.,-0.84881193451618));
#28102=DIRECTION('center_axis',(-0.772541698292714,0.,-0.634964033941301));
#28103=DIRECTION('ref_axis',(-0.634964033941301,0.,0.772541698292714));
#28104=DIRECTION('',(-0.634964033941407,0.,0.772541698292626));
#28105=DIRECTION('',(0.,-1.,0.));
#28106=DIRECTION('',(0.634964033941407,0.,-0.772541698292626));
#28107=DIRECTION('center_axis',(-0.581877193327018,0.,-0.813276663802591));
#28108=DIRECTION('ref_axis',(-0.813276663802591,0.,0.581877193327018));
#28109=DIRECTION('',(-0.813276663802456,0.,0.581877193327206));
#28110=DIRECTION('',(0.,-1.,0.));
#28111=DIRECTION('',(0.813276663802456,0.,-0.581877193327206));
#28112=DIRECTION('center_axis',(-0.470745247127108,0.,-0.882269183586981));
#28113=DIRECTION('ref_axis',(-0.882269183586981,0.,0.470745247127108));
#28114=DIRECTION('',(-0.882269183586787,0.,0.470745247127471));
#28115=DIRECTION('',(0.,-1.,0.));
#28116=DIRECTION('',(0.882269183586787,0.,-0.470745247127471));
#28117=DIRECTION('center_axis',(0.,1.,0.));
#28118=DIRECTION('ref_axis',(0.902585284349861,0.,-0.430511096808295));
#28119=DIRECTION('center_axis',(0.,-1.,0.));
#28120=DIRECTION('ref_axis',(0.902585284349705,0.,-0.430511096808622));
#28121=DIRECTION('',(0.,-1.,0.));
#28122=DIRECTION('center_axis',(0.,1.,0.));
#28123=DIRECTION('ref_axis',(0.902585284349705,0.,-0.430511096808622));
#28124=DIRECTION('center_axis',(0.,1.,0.));
#28125=DIRECTION('ref_axis',(0.902585284349861,0.,-0.430511096808295));
#28126=DIRECTION('center_axis',(0.,1.,0.));
#28127=DIRECTION('ref_axis',(0.902585284349705,0.,-0.430511096808622));
#28128=DIRECTION('center_axis',(0.,-1.,0.));
#28129=DIRECTION('ref_axis',(0.902585284349705,0.,-0.430511096808622));
#28130=DIRECTION('center_axis',(0.,1.,0.));
#28131=DIRECTION('ref_axis',(1.,0.,0.));
#28132=DIRECTION('',(-0.430511096808717,0.,0.902585284349659));
#28133=DIRECTION('center_axis',(0.,-1.,0.));
#28134=DIRECTION('ref_axis',(-0.902585284349714,0.,0.430511096808602));
#28135=DIRECTION('',(0.902585284349659,0.,-0.430511096808717));
#28136=DIRECTION('center_axis',(0.,1.,0.));
#28137=DIRECTION('ref_axis',(0.902585284349705,0.,-0.430511096808622));
#28138=DIRECTION('center_axis',(0.,1.,0.));
#28139=DIRECTION('ref_axis',(0.902585284349705,0.,-0.430511096808622));
#28140=DIRECTION('center_axis',(0.,1.,0.));
#28141=DIRECTION('ref_axis',(0.902585284349705,0.,-0.430511096808622));
#28142=DIRECTION('',(-0.730368754817616,0.,0.683053059422301));
#28143=DIRECTION('center_axis',(0.,1.,0.));
#28144=DIRECTION('ref_axis',(0.902585284349705,0.,-0.430511096808622));
#28145=DIRECTION('center_axis',(0.,1.,0.));
#28146=DIRECTION('ref_axis',(0.902585284349861,0.,-0.430511096808295));
#28147=DIRECTION('center_axis',(0.,-1.,0.));
#28148=DIRECTION('ref_axis',(0.902585284349705,0.,-0.430511096808622));
#28149=DIRECTION('',(0.,-1.,0.));
#28150=DIRECTION('center_axis',(0.,1.,0.));
#28151=DIRECTION('ref_axis',(0.902585284349861,0.,-0.430511096808295));
#28152=DIRECTION('',(0.,1.,0.));
#28153=DIRECTION('center_axis',(0.,-1.,0.));
#28154=DIRECTION('ref_axis',(0.902585284349705,0.,-0.430511096808622));
#28155=DIRECTION('center_axis',(-0.683053059422266,0.,-0.730368754817649));
#28156=DIRECTION('ref_axis',(-0.730368754817649,0.,0.683053059422266));
#28157=DIRECTION('',(0.730368754817616,0.,-0.683053059422301));
#28158=DIRECTION('center_axis',(0.,1.,0.));
#28159=DIRECTION('ref_axis',(0.902585284349861,0.,-0.430511096808295));
#28160=DIRECTION('center_axis',(0.,-1.,0.));
#28161=DIRECTION('ref_axis',(0.902585284349705,0.,-0.430511096808622));
#28162=DIRECTION('center_axis',(0.902585284349863,0.,0.430511096808291));
#28163=DIRECTION('ref_axis',(0.,-1.,0.));
#28164=DIRECTION('',(0.430511096808717,0.,-0.902585284349659));
#28165=DIRECTION('',(0.,1.,0.));
#28166=DIRECTION('center_axis',(0.,1.,0.));
#28167=DIRECTION('ref_axis',(-0.902585284349861,0.,0.430511096808295));
#28168=DIRECTION('center_axis',(0.,1.,0.));
#28169=DIRECTION('ref_axis',(-0.902585284349714,0.,0.430511096808602));
#28170=DIRECTION('',(0.,1.,0.));
#28171=DIRECTION('center_axis',(-0.430511096808291,0.,-0.902585284349863));
#28172=DIRECTION('ref_axis',(-0.902585284349863,0.,0.430511096808291));
#28173=DIRECTION('',(-0.902585284349659,0.,0.430511096808717));
#28174=DIRECTION('center_axis',(0.,1.,0.));
#28175=DIRECTION('ref_axis',(0.902585284349861,0.,-0.430511096808295));
#28176=DIRECTION('center_axis',(0.,-1.,0.));
#28177=DIRECTION('ref_axis',(0.902585284349705,0.,-0.430511096808622));
#28178=DIRECTION('center_axis',(0.,1.,0.));
#28179=DIRECTION('ref_axis',(1.,0.,0.));
#28180=DIRECTION('axis',(0.,0.,1.));
#28181=DIRECTION('refdir',(1.,0.,0.));
#28182=DIRECTION('center_axis',(4.55032717710333E-17,-1.,1.51850909121962E-32));
#28183=DIRECTION('ref_axis',(-0.770184521566975,0.,0.637821136948792));
#28184=DIRECTION('center_axis',(-4.55032717710333E-17,1.,-1.51850909121962E-32));
#28185=DIRECTION('ref_axis',(0.637821136951873,2.90229485360305E-17,0.770184521564424));
#28186=DIRECTION('center_axis',(0.637821136948792,2.90229485358903E-17,
0.770184521566975));
#28187=DIRECTION('ref_axis',(0.770184521566975,0.,-0.637821136948792));
#28188=DIRECTION('center_axis',(4.55032717710333E-17,-1.,1.51850909121962E-32));
#28189=DIRECTION('ref_axis',(0.637821136951568,2.90229485360166E-17,0.770184521564676));
#28190=DIRECTION('center_axis',(-4.55032717710333E-17,1.,-1.51850909121962E-32));
#28191=DIRECTION('ref_axis',(0.637821136951873,2.90229485360305E-17,0.770184521564424));
#28192=DIRECTION('center_axis',(4.55032717710333E-17,-1.,1.51850909121962E-32));
#28193=DIRECTION('ref_axis',(-0.637821136948792,-2.90229485358903E-17,-0.770184521566975));
#28194=DIRECTION('center_axis',(4.55032717710333E-17,-1.,1.51850909121962E-32));
#28195=DIRECTION('ref_axis',(0.637821136951873,2.90229485360305E-17,0.770184521564424));
#28196=DIRECTION('',(4.55032717710333E-17,-1.,1.51850909121962E-32));
#28197=DIRECTION('center_axis',(4.55032717710333E-17,-1.,1.51850909121962E-32));
#28198=DIRECTION('ref_axis',(0.637821136951873,2.90229485360305E-17,0.770184521564424));
#28199=DIRECTION('center_axis',(4.55032717710333E-17,-1.,1.51850909121962E-32));
#28200=DIRECTION('ref_axis',(-0.637821136948792,-2.90229485358903E-17,-0.770184521566975));
#28201=DIRECTION('center_axis',(4.55032717710333E-17,-1.,1.51850909121962E-32));
#28202=DIRECTION('ref_axis',(-0.637821136948792,-2.90229485358903E-17,-0.770184521566975));
#28203=DIRECTION('center_axis',(4.55032717710333E-17,-1.,1.51850909121962E-32));
#28204=DIRECTION('ref_axis',(-0.770184521566975,0.,0.637821136948792));
#28205=DIRECTION('center_axis',(-4.55032717710333E-17,1.,-1.51850909121962E-32));
#28206=DIRECTION('ref_axis',(0.637821136951568,2.90229485360166E-17,0.770184521564676));
#28207=DIRECTION('center_axis',(0.637821136948792,2.90229485358903E-17,
0.770184521566975));
#28208=DIRECTION('ref_axis',(0.770184521566975,0.,-0.637821136948792));
#28209=DIRECTION('center_axis',(-4.55032717710333E-17,1.,-1.51850909121962E-32));
#28210=DIRECTION('ref_axis',(0.770184521566975,3.50459155987053E-17,-0.637821136948792));
#28211=DIRECTION('center_axis',(4.55032717710333E-17,-1.,1.51850909121962E-32));
#28212=DIRECTION('ref_axis',(-0.637821136948792,-2.90229485358903E-17,-0.770184521566975));
#28213=DIRECTION('center_axis',(4.55032717710333E-17,-1.,1.51850909121962E-32));
#28214=DIRECTION('ref_axis',(-0.637821136948792,-2.90229485358903E-17,-0.770184521566975));
#28215=DIRECTION('',(-4.55032717710333E-17,1.,-1.51850909121962E-32));
#28216=DIRECTION('axis',(0.,0.,1.));
#28217=DIRECTION('refdir',(1.,0.,0.));
#28218=DIRECTION('center_axis',(1.,5.1420277733694E-16,-1.0522467400333E-14));
#28219=DIRECTION('ref_axis',(-1.0522467400333E-14,1.06077175752244E-14,
-1.));
#28220=DIRECTION('',(-1.00001914094642E-12,1.00002200370999E-12,1.));
#28221=DIRECTION('',(-9.47915311079142E-15,-1.,1.E-14));
#28222=DIRECTION('',(1.00001914094642E-12,-9.99999999998997E-13,-1.));
#28223=DIRECTION('',(-9.47915311079142E-15,-1.,1.E-14));
#28224=DIRECTION('center_axis',(1.,5.2084688920845E-16,-1.0522467400333E-14));
#28225=DIRECTION('ref_axis',(-1.0522467400333E-14,1.01548957588061E-14,
-1.));
#28226=DIRECTION('',(-9.56631913100564E-15,9.99999999999985E-15,1.));
#28227=DIRECTION('',(-9.47915311079142E-15,-1.,1.E-14));
#28228=DIRECTION('',(-9.56631913100564E-15,9.99999999999985E-15,1.));
#28229=DIRECTION('',(-9.47915311079142E-15,-1.,1.E-14));
#28230=DIRECTION('center_axis',(0.,-4.29362650667545E-31,1.));
#28231=DIRECTION('ref_axis',(4.28756753891971E-16,-1.,-4.29362650667545E-31));
#28232=DIRECTION('',(-9.99999999999976E-15,-1.04336808689941E-14,1.));
#28233=DIRECTION('center_axis',(-1.99999999991998E-11,2.E-11,1.));
#28234=DIRECTION('ref_axis',(-1.99995712428458E-11,-1.,1.99999999996E-11));
#28235=DIRECTION('center_axis',(-1.99999999991998E-11,2.E-11,1.));
#28236=DIRECTION('ref_axis',(-1.99995712428458E-11,-1.,1.99999999996E-11));
#28237=DIRECTION('center_axis',(-4.5961454925099E-16,1.,6.61092274672771E-17));
#28238=DIRECTION('ref_axis',(-1.05885766278003E-14,6.61092274672722E-17,
-1.));
#28239=DIRECTION('',(1.,-9.54038545074888E-15,9.9999999999998E-15));
#28240=DIRECTION('',(-1.,9.54038545074888E-15,-9.9999999999998E-15));
#28241=DIRECTION('center_axis',(-2.43331626335218E-16,4.46289580949563E-15,
1.));
#28242=DIRECTION('ref_axis',(1.,3.89820370584558E-15,2.43331626335201E-16));
#28243=DIRECTION('',(-1.,9.99485333130104E-13,-9.99628143109513E-13));
#28244=DIRECTION('',(-9.99479153109778E-13,-1.,1.0044628958085E-12));
#28245=DIRECTION('',(1.,-9.99466108488984E-13,1.00024333162532E-12));
#28246=DIRECTION('center_axis',(-5.3389151001178E-16,1.,6.61092274672815E-17));
#28247=DIRECTION('ref_axis',(-9.50035731417012E-15,6.61092274672764E-17,
-1.));
#28248=DIRECTION('',(-9.99999999998985E-13,-1.00108821931263E-12,1.));
#28249=DIRECTION('',(1.,-9.99466108488984E-13,1.00024333162532E-12));
#28250=DIRECTION('center_axis',(-1.0522467400333E-14,-4.46289580949556E-15,
-1.));
#28251=DIRECTION('ref_axis',(1.,-6.86759532082262E-15,-1.0522467400333E-14));
#28252=DIRECTION('',(9.99479153109778E-13,1.,-1.0044628958085E-12));
#28253=DIRECTION('',(1.,-9.99466108488984E-13,1.00024333162532E-12));
#28254=DIRECTION('center_axis',(5.33891510011771E-16,-1.,2.20037109950003E-17));
#28255=DIRECTION('ref_axis',(-1.,-5.33891510011771E-16,1.0522467400333E-14));
#28256=DIRECTION('',(9.99999999998993E-13,-1.00002200370999E-12,-1.));
#28257=DIRECTION('center_axis',(1.,5.33891510011885E-16,-1.0522467400333E-14));
#28258=DIRECTION('ref_axis',(-1.0522467400333E-14,1.08319082541355E-14,
-1.));
#28259=DIRECTION('axis',(0.,0.,1.));
#28260=DIRECTION('refdir',(1.,0.,0.));
#28261=DIRECTION('center_axis',(6.02124417213197E-17,-1.,3.1081360155032E-32));
#28262=DIRECTION('ref_axis',(1.,6.02124417213197E-17,1.69633130794335E-33));
#28263=DIRECTION('center_axis',(-6.02124417213197E-17,1.,-3.1081360155032E-32));
#28264=DIRECTION('ref_axis',(1.,6.02124417213197E-17,1.69633130794335E-33));
#28265=DIRECTION('',(0.70699152335979,0.707222020229435,8.65814906106877E-17));
#28266=DIRECTION('center_axis',(-8.38023770707909E-12,-1.,3.10813601550178E-32));
#28267=DIRECTION('ref_axis',(1.,-8.38023770707909E-12,1.69633130820382E-33));
#28268=DIRECTION('center_axis',(-6.02124417213197E-17,1.,-3.1081360155032E-32));
#28269=DIRECTION('ref_axis',(1.,6.02124417213197E-17,1.69633130794335E-33));
#28270=DIRECTION('center_axis',(-6.02124417213197E-17,1.,-3.1081360155032E-32));
#28271=DIRECTION('ref_axis',(-1.,-6.02124417213197E-17,-1.69633130794335E-33));
#28272=DIRECTION('',(6.02124417213197E-17,-1.,3.1081360155032E-32));
#28273=DIRECTION('center_axis',(-6.02124417213197E-17,1.,-3.1081360155032E-32));
#28274=DIRECTION('ref_axis',(-1.,-6.02124417213197E-17,-1.69633130794335E-33));
#28275=DIRECTION('center_axis',(-6.02124417213197E-17,1.,-3.1081360155032E-32));
#28276=DIRECTION('ref_axis',(-1.69633130794335E-33,3.1081360155032E-32,
1.));
#28277=DIRECTION('center_axis',(-6.02124417213197E-17,1.,-3.1081360155032E-32));
#28278=DIRECTION('ref_axis',(0.,0.,-1.));
#28279=DIRECTION('center_axis',(-6.02124417213197E-17,1.,-3.1081360155032E-32));
#28280=DIRECTION('ref_axis',(-1.,-6.02124417213197E-17,7.31030425583873E-12));
#28281=DIRECTION('center_axis',(6.02123954565766E-17,-1.,-6.80180522852632E-12));
#28282=DIRECTION('ref_axis',(-1.,-6.02124417213198E-17,6.80183298410194E-12));
#28283=DIRECTION('center_axis',(6.02124417213197E-17,-1.,3.1081360155032E-32));
#28284=DIRECTION('ref_axis',(-1.,-6.02124417213197E-17,-1.69633130794335E-33));
#28285=DIRECTION('center_axis',(-6.02124417213197E-17,1.,-3.1081360155032E-32));
#28286=DIRECTION('ref_axis',(-1.,-6.02124417213197E-17,-1.69633130794335E-33));
#28287=DIRECTION('center_axis',(-6.02124417213197E-17,1.,-3.1081360155032E-32));
#28288=DIRECTION('ref_axis',(0.,0.,-1.));
#28289=DIRECTION('center_axis',(-6.02124417213197E-17,1.,-3.1081360155032E-32));
#28290=DIRECTION('ref_axis',(-7.31034016801343E-12,-4.40204512689686E-28,
-1.));
#28291=DIRECTION('center_axis',(-6.8017450160846E-12,-1.,4.62649708883395E-23));
#28292=DIRECTION('ref_axis',(-6.80186646086628E-12,-4.09588069284889E-28,
-1.));
#28293=DIRECTION('center_axis',(6.02124417213197E-17,-1.,3.1081360155032E-32));
#28294=DIRECTION('ref_axis',(-1.,-6.02124417213197E-17,-1.69633130794335E-33));
#28295=DIRECTION('center_axis',(-6.02124417213197E-17,1.,-3.1081360155032E-32));
#28296=DIRECTION('ref_axis',(-1.,-6.02124417213197E-17,-1.69633130794335E-33));
#28297=DIRECTION('center_axis',(-6.02124417213197E-17,1.,-3.1081360155032E-32));
#28298=DIRECTION('ref_axis',(0.,0.,-1.));
#28299=DIRECTION('center_axis',(-6.02124417213197E-17,1.,-3.1081360155032E-32));
#28300=DIRECTION('ref_axis',(1.,6.02124417213197E-17,1.69633130794335E-33));
#28301=DIRECTION('center_axis',(6.02123954559324E-17,-1.,6.80180522852632E-12));
#28302=DIRECTION('ref_axis',(1.,6.02124417213198E-17,6.80192769320624E-12));
#28303=DIRECTION('center_axis',(6.02124417213197E-17,-1.,3.1081360155032E-32));
#28304=DIRECTION('ref_axis',(1.,6.02124417213197E-17,1.22464679914735E-16));
#28305=DIRECTION('center_axis',(-6.02124417213197E-17,1.,-3.1081360155032E-32));
#28306=DIRECTION('ref_axis',(-1.,-6.02124417213197E-17,-1.69633130794335E-33));
#28307=DIRECTION('center_axis',(-6.02124417213197E-17,1.,-3.1081360155032E-32));
#28308=DIRECTION('ref_axis',(-1.,-6.02124417213197E-17,-1.69633130794335E-33));
#28309=DIRECTION('center_axis',(-6.02124417213197E-17,1.,-3.1081360155032E-32));
#28310=DIRECTION('ref_axis',(0.,0.,1.));
#28311=DIRECTION('center_axis',(-6.02124417213197E-17,1.,-3.1081360155032E-32));
#28312=DIRECTION('ref_axis',(-7.31034016801343E-12,-4.40142349969376E-28,
1.));
#28313=DIRECTION('center_axis',(-6.8017450160846E-12,-1.,-4.62649708261767E-23));
#28314=DIRECTION('ref_axis',(-6.80186646086628E-12,-4.09525906487E-28,1.));
#28315=DIRECTION('center_axis',(6.02124417213197E-17,-1.,3.1081360155032E-32));
#28316=DIRECTION('ref_axis',(-1.,-6.02124417213197E-17,-1.69633130794335E-33));
#28317=DIRECTION('center_axis',(-6.02124417213197E-17,1.,-3.1081360155032E-32));
#28318=DIRECTION('ref_axis',(-1.,-6.02124417213197E-17,-1.69633130794335E-33));
#28319=DIRECTION('center_axis',(-6.02124417213197E-17,1.,-3.1081360155032E-32));
#28320=DIRECTION('ref_axis',(0.,0.,-1.));
#28321=DIRECTION('center_axis',(6.02124417213197E-17,-1.,3.1081360155032E-32));
#28322=DIRECTION('ref_axis',(1.,6.02124417213197E-17,1.69633130794335E-33));
#28323=DIRECTION('center_axis',(1.,6.02124417213197E-17,0.));
#28324=DIRECTION('ref_axis',(0.,0.,1.));
#28325=DIRECTION('center_axis',(-6.02124211725949E-17,1.,-4.53300889872937E-12));
#28326=DIRECTION('ref_axis',(1.,6.02124417213197E-17,4.53313136340929E-12));
#28327=DIRECTION('center_axis',(6.02124417213197E-17,-1.,3.1081360155032E-32));
#28328=DIRECTION('ref_axis',(1.,6.02124417213197E-17,1.69633130794335E-33));
#28329=DIRECTION('center_axis',(0.,0.,1.));
#28330=DIRECTION('ref_axis',(0.0108223376335956,-0.999941436789247,0.));
#28331=DIRECTION('center_axis',(0.0407206959932429,-0.0871557427495498,
-0.995362095633343));
#28332=DIRECTION('ref_axis',(0.999164217135634,6.02779468193653E-17,0.0408762424365959));
#28333=DIRECTION('center_axis',(0.995362095633343,-0.0871557427495499,-0.0407206959932438));
#28334=DIRECTION('ref_axis',(0.0408762424365968,9.94030957902627E-18,0.999164217135634));
#28335=DIRECTION('center_axis',(-0.995362095633343,-0.08715574274955,-0.0407206959932438));
#28336=DIRECTION('ref_axis',(0.0408762424365968,-4.74217326228398E-18,-0.999164217135634));
#28337=DIRECTION('center_axis',(-0.0407206959932429,-0.0871557427495498,
-0.995362095633343));
#28338=DIRECTION('ref_axis',(0.999164217135634,5.8550611285046E-17,-0.0408762424365959));
#28339=DIRECTION('center_axis',(-0.0407206959932429,-0.0871557427495498,
0.995362095633343));
#28340=DIRECTION('ref_axis',(-0.999164217135634,-5.8550611285046E-17,-0.0408762424365959));
#28341=DIRECTION('center_axis',(-0.995362095633343,-0.08715574274955,0.0407206959932438));
#28342=DIRECTION('ref_axis',(-0.0408762424365968,4.74217326228398E-18,-0.999164217135634));
#28343=DIRECTION('center_axis',(0.995362095633343,-0.0871557427495499,0.0407206959932438));
#28344=DIRECTION('ref_axis',(-0.0408762424365968,-9.94030957902627E-18,
0.999164217135634));
#28345=DIRECTION('center_axis',(0.0407206959932429,-0.0871557427495498,
0.995362095633343));
#28346=DIRECTION('ref_axis',(-0.999164217135634,-6.02779468193653E-17,0.0408762424365959));
#28347=DIRECTION('center_axis',(-6.02124417213197E-17,1.,-3.1081360155032E-32));
#28348=DIRECTION('ref_axis',(-1.,-6.02124417213197E-17,-1.69633130794335E-33));
#28349=DIRECTION('center_axis',(-6.02124417213197E-17,1.,-3.1081360155032E-32));
#28350=DIRECTION('ref_axis',(-1.,-6.02124417213197E-17,-1.69633130794335E-33));
#28351=DIRECTION('',(-0.0348994967025007,-0.999390827019096,4.27395569285715E-18));
#28352=DIRECTION('center_axis',(-6.02124417213197E-17,1.,-3.1081360155032E-32));
#28353=DIRECTION('ref_axis',(0.999164217135713,6.01621171943121E-17,-0.0408762424346739));
#28354=DIRECTION('',(0.0035625992711232,0.996194698091663,-0.0870828994722507));
#28355=DIRECTION('',(0.0870828994722507,0.996194698091663,-0.00356259927112407));
#28356=DIRECTION('center_axis',(0.0407206959913409,-0.0871557427476582,
-0.995362095633586));
#28357=DIRECTION('ref_axis',(5.77166398093136E-17,-0.99618836566326,0.0872280924769298));
#28358=DIRECTION('center_axis',(0.0407206959913409,-0.0871557427476582,
0.995362095633586));
#28359=DIRECTION('ref_axis',(-0.905991774445375,-0.423295292481881,5.86723486602494E-17));
#28360=DIRECTION('',(0.00356259927112393,0.996194698091663,0.0870828994722507));
#28361=DIRECTION('center_axis',(-6.02124417213197E-17,1.,-3.1081360155032E-32));
#28362=DIRECTION('ref_axis',(0.0408762424346715,2.46125836538422E-18,0.999164217135713));
#28363=DIRECTION('',(0.0870828994722507,0.996194698091663,0.00356259927112347));
#28364=DIRECTION('center_axis',(-0.0407206959913409,-0.0871557427476582,
0.995362095633586));
#28365=DIRECTION('ref_axis',(-0.905991774445375,0.423295292481881,-5.86723486602494E-17));
#28366=DIRECTION('',(-0.00356259927112332,0.996194698091663,0.0870828994722507));
#28367=DIRECTION('center_axis',(0.995362095633586,-0.0871557427476581,0.0407206959913419));
#28368=DIRECTION('ref_axis',(-0.0872280924769297,-0.99618836566326,-2.68621612590795E-18));
#28369=DIRECTION('center_axis',(0.995362095633586,-0.0871557427476581,-0.0407206959913419));
#28370=DIRECTION('ref_axis',(-0.0872280924769297,-0.99618836566326,2.68621612590795E-18));
#28371=DIRECTION('center_axis',(-0.995362095633586,-0.0871557427476583,
-0.0407206959913419));
#28372=DIRECTION('ref_axis',(3.56814972436615E-17,-0.42329529248189,0.905991774445371));
#28373=DIRECTION('',(-0.0870828994722508,0.996194698091663,-0.00356259927112347));
#28374=DIRECTION('center_axis',(-0.995362095633586,-0.0871557427476583,
0.0407206959913419));
#28375=DIRECTION('ref_axis',(-3.56814972436615E-17,0.42329529248189,0.905991774445371));
#28376=DIRECTION('',(-0.0870828994722508,0.996194698091663,0.00356259927112407));
#28377=DIRECTION('center_axis',(-6.02124417213197E-17,1.,-3.1081360155032E-32));
#28378=DIRECTION('ref_axis',(-0.999164217135713,-6.01621171943121E-17,0.0408762424346739));
#28379=DIRECTION('center_axis',(-6.02124417213197E-17,1.,-3.1081360155032E-32));
#28380=DIRECTION('ref_axis',(-0.0408762424346715,-2.46125836538422E-18,
-0.999164217135713));
#28381=DIRECTION('',(-0.00356259927112405,0.996194698091663,-0.0870828994722507));
#28382=DIRECTION('center_axis',(-0.0407206959913409,-0.0871557427476582,
-0.995362095633586));
#28383=DIRECTION('ref_axis',(6.27251844107897E-17,-0.99618836566326,0.0872280924769298));
#28384=DIRECTION('center_axis',(6.02124417213197E-17,-1.,3.1081360155032E-32));
#28385=DIRECTION('ref_axis',(-1.,-6.02124417213197E-17,-1.69633130794335E-33));
#28386=DIRECTION('',(0.88294759285893,-0.469471562785886,1.08129894340955E-16));
#28387=DIRECTION('center_axis',(-6.02124417213197E-17,1.,-3.1081360155032E-32));
#28388=DIRECTION('ref_axis',(-1.,-6.02124417213197E-17,-1.69633130794335E-33));
#28389=DIRECTION('center_axis',(-6.02124417213197E-17,1.,-3.1081360155032E-32));
#28390=DIRECTION('ref_axis',(-1.,-6.02124417213197E-17,-1.69633130794335E-33));
#28391=DIRECTION('',(6.02124417213197E-17,-1.,3.1081360155032E-32));
#28392=DIRECTION('center_axis',(-6.02124417213197E-17,1.,-3.1081360155032E-32));
#28393=DIRECTION('ref_axis',(-1.,-6.02124417213197E-17,-1.69633130794335E-33));
#28394=DIRECTION('center_axis',(-6.02124417213197E-17,1.,-3.1081360155032E-32));
#28395=DIRECTION('ref_axis',(-1.69633130794335E-33,3.1081360155032E-32,
1.));
#28396=DIRECTION('center_axis',(-6.02124417213197E-17,1.,-3.1081360155032E-32));
#28397=DIRECTION('ref_axis',(-1.,-6.02124417213197E-17,-1.69633130794335E-33));
#28398=DIRECTION('',(-0.403628089275423,-0.914923147345104,4.94301847577109E-17));
#28399=DIRECTION('',(4.64905891561784E-16,1.,1.04083408558609E-16));
#28400=DIRECTION('',(-1.,4.64905891561784E-16,-7.19835576014173E-30));
#28401=DIRECTION('',(4.64905891561784E-16,1.,1.04083408558609E-16));
#28402=DIRECTION('',(-1.,4.64905891561784E-16,-7.19835576014173E-30));
#28403=DIRECTION('',(4.64905891561784E-16,1.,1.04083408558609E-16));
#28404=DIRECTION('',(-1.,4.64905891561784E-16,-7.19835576014173E-30));
#28405=DIRECTION('',(4.64905891561784E-16,1.,1.04083408558609E-16));
#28406=DIRECTION('',(-1.,4.64905891561784E-16,-7.19835576014173E-30));
#28407=DIRECTION('',(4.64905891561784E-16,1.,1.04083408558609E-16));
#28408=DIRECTION('',(-1.,4.64905891561784E-16,-7.19835576014173E-30));
#28409=DIRECTION('',(4.64905891561784E-16,1.,1.04083408558609E-16));
#28410=DIRECTION('',(-1.,4.64905891561784E-16,-7.19835576014173E-30));
#28411=DIRECTION('',(-3.23074900165921E-13,0.999999999999999,1.18291379027158E-15));
#28412=DIRECTION('',(-1.,-3.22186721746221E-13,4.00301953561515E-17));
#28413=DIRECTION('',(4.64905891561784E-16,1.,1.04083408558609E-16));
#28414=DIRECTION('',(-1.,4.64905891561784E-16,-7.19835576014173E-30));
#28415=DIRECTION('',(4.64905891561784E-16,1.,1.04083408558609E-16));
#28416=DIRECTION('',(-1.,4.64905891561784E-16,-7.19835576014173E-30));
#28417=DIRECTION('',(4.64905891561784E-16,1.,1.04083408558609E-16));
#28418=DIRECTION('',(-1.,4.64905891561784E-16,-7.19835576014173E-30));
#28419=DIRECTION('',(4.64905891561784E-16,1.,1.04083408558609E-16));
#28420=DIRECTION('',(-1.,4.64905891561784E-16,-7.19835576014173E-30));
#28421=DIRECTION('',(4.64905891561784E-16,1.,1.04083408558609E-16));
#28422=DIRECTION('',(-1.,4.64905891561784E-16,-7.19835576014173E-30));
#28423=DIRECTION('',(4.64905891561784E-16,1.,1.04083408558609E-16));
#28424=DIRECTION('',(-1.,4.64905891561784E-16,-7.19835576014173E-30));
#28425=DIRECTION('',(4.64905891561784E-16,1.,1.04083408558609E-16));
#28426=DIRECTION('',(-1.,4.64905891561784E-16,-7.19835576014173E-30));
#28427=DIRECTION('',(4.64905891561784E-16,1.,1.04083408558609E-16));
#28428=DIRECTION('',(-1.,4.64905891561784E-16,-7.19835576014173E-30));
#28429=DIRECTION('',(4.64905891561784E-16,1.,1.04083408558609E-16));
#28430=DIRECTION('',(-1.,4.64905891561784E-16,-7.19835576014173E-30));
#28431=DIRECTION('',(4.64905891561784E-16,1.,1.04083408558609E-16));
#28432=DIRECTION('',(-1.,4.64905891561784E-16,-7.19835576014173E-30));
#28433=DIRECTION('',(4.64905891561784E-16,1.,1.04083408558609E-16));
#28434=DIRECTION('',(-1.,4.64905891561784E-16,-7.19835576014173E-30));
#28435=DIRECTION('',(4.64905891561784E-16,1.,1.04083408558609E-16));
#28436=DIRECTION('',(-1.,4.64905891561784E-16,-7.19835576014173E-30));
#28437=DIRECTION('',(4.64905891561784E-16,1.,1.04083408558609E-16));
#28438=DIRECTION('',(-1.,4.64905891561784E-16,-7.19835576014173E-30));
#28439=DIRECTION('',(4.64905891561784E-16,1.,1.04083408558609E-16));
#28440=DIRECTION('',(-1.,4.64905891561784E-16,-7.19835576014173E-30));
#28441=DIRECTION('',(4.64905891561784E-16,1.,1.04083408558609E-16));
#28442=DIRECTION('',(-1.,4.64905891561784E-16,-7.19835576014173E-30));
#28443=DIRECTION('',(4.64905891561784E-16,1.,1.04083408558609E-16));
#28444=DIRECTION('',(-1.,4.64905891561784E-16,-7.19835576014173E-30));
#28445=DIRECTION('',(4.64905891561784E-16,1.,1.04083408558609E-16));
#28446=DIRECTION('',(-1.,4.64905891561784E-16,-7.19835576014173E-30));
#28447=DIRECTION('',(4.64905891561784E-16,1.,1.04083408558609E-16));
#28448=DIRECTION('',(-1.,4.64905891561784E-16,-7.19835576014173E-30));
#28449=DIRECTION('',(4.64905891561784E-16,1.,1.04083408558609E-16));
#28450=DIRECTION('',(-1.,4.64905891561784E-16,-7.19835576014173E-30));
#28451=DIRECTION('',(4.64905891561784E-16,1.,1.04083408558609E-16));
#28452=DIRECTION('',(-1.,4.64905891561784E-16,-7.19835576014173E-30));
#28453=DIRECTION('',(4.64905891561784E-16,1.,1.04083408558609E-16));
#28454=DIRECTION('',(-1.,4.64905891561784E-16,-7.19835576014173E-30));
#28455=DIRECTION('',(4.64905891561784E-16,1.,1.04083408558609E-16));
#28456=DIRECTION('',(-1.,4.64905891561784E-16,-7.19835576014173E-30));
#28457=DIRECTION('',(4.64905891561784E-16,1.,1.04083408558609E-16));
#28458=DIRECTION('',(-1.,4.64905891561784E-16,-7.19835576014173E-30));
#28459=DIRECTION('',(4.64905891561784E-16,1.,1.04083408558609E-16));
#28460=DIRECTION('',(-1.,4.64905891561784E-16,-7.19835576014173E-30));
#28461=DIRECTION('',(4.64905891561784E-16,1.,1.04083408558609E-16));
#28462=DIRECTION('',(-1.,4.64905891561784E-16,-7.19835576014173E-30));
#28463=DIRECTION('',(4.64905891561784E-16,1.,1.04083408558609E-16));
#28464=DIRECTION('',(-1.,4.64905891561784E-16,-7.19835576014173E-30));
#28465=DIRECTION('',(0.00113622352562814,0.999999354497841,1.18196693116941E-15));
#28466=DIRECTION('',(-0.999999354497842,0.00113622352562864,8.34010247969466E-16));
#28467=DIRECTION('',(4.64905891561784E-16,1.,1.04083408558609E-16));
#28468=DIRECTION('',(-1.,4.64905891561784E-16,-7.19835576014173E-30));
#28469=DIRECTION('',(-0.0039046348050254,0.999992376884463,1.18702298187498E-15));
#28470=DIRECTION('',(-0.999992376884464,-0.00390463480502557,1.05007074792371E-15));
#28471=CARTESIAN_POINT('',(0.,0.,0.));
#28472=CARTESIAN_POINT('',(0.,0.,0.));
#28473=CARTESIAN_POINT('Origin',(-4.50826289289608E-17,-0.006725,1.13636778952413E-32));
#28474=CARTESIAN_POINT('',(0.00594967542911254,-0.00700000000001,-0.00492716828293579));
#28475=CARTESIAN_POINT('Origin',(-4.50701155292233E-17,-0.00700000000001,
1.13678537952423E-32));
#28476=CARTESIAN_POINT('',(0.00616147617254346,-0.00672500000001,-0.00510256909559671));
#28477=CARTESIAN_POINT('Origin',(0.00594967542910484,-0.006725,-0.00492716828292942));
#28478=CARTESIAN_POINT('',(0.00510256909560437,-0.00672500000001,0.00616147617253713));
#28479=CARTESIAN_POINT('Origin',(-4.50826289289603E-17,-0.00672500000001,
1.13636778952415E-32));
#28480=CARTESIAN_POINT('Origin',(-4.50826289289603E-17,-0.00672500000001,
1.13636778952415E-32));
#28481=CARTESIAN_POINT('Origin',(-4.51838737086513E-17,-0.0045,1.13298910679617E-32));
#28482=CARTESIAN_POINT('',(0.00510256909560437,-0.00227500000001,0.00616147617253713));
#28483=CARTESIAN_POINT('',(0.00510256909559029,-0.0045,0.0061614761725358));
#28484=CARTESIAN_POINT('',(0.00616147617254346,-0.00227500000001001,-0.00510256909559671));
#28485=CARTESIAN_POINT('Origin',(-4.52851184883414E-17,-0.00227500000001001,
1.12961042406822E-32));
#28486=CARTESIAN_POINT('Origin',(-4.52851184883414E-17,-0.00227500000001001,
1.12961042406822E-32));
#28487=CARTESIAN_POINT('Origin',(-0.00451789972005399,-0.007,-0.00545547369443274));
#28488=CARTESIAN_POINT('',(0.0039332303445175,-0.00700000000001,0.00474947121632968));
#28489=CARTESIAN_POINT('Origin',(-4.50701155292233E-17,-0.00700000000001,
1.13678537952423E-32));
#28490=CARTESIAN_POINT('Origin',(-4.52851184883419E-17,-0.002275,1.1296104240682E-32));
#28491=CARTESIAN_POINT('',(0.00594967542911254,-0.00200000000001001,-0.00492716828293579));
#28492=CARTESIAN_POINT('Origin',(0.00594967542910484,-0.002275,-0.00492716828292942));
#28493=CARTESIAN_POINT('Origin',(-4.52976318880785E-17,-0.00200000000001001,
1.12919283406813E-32));
#28494=CARTESIAN_POINT('Origin',(-0.00451789972005399,-0.002,-0.00545547369443274));
#28495=CARTESIAN_POINT('',(0.0039332303445175,-0.00200000000001001,0.00474947121632968));
#28496=CARTESIAN_POINT('Origin',(-4.52976318880785E-17,-0.00200000000001001,
1.12919283406813E-32));
#28497=CARTESIAN_POINT('Origin',(-4.51838737086513E-17,-0.0045,1.13298910679617E-32));
#28498=CARTESIAN_POINT('',(0.0039332303445175,-0.0045,0.00474947121632968));
#28499=CARTESIAN_POINT('',(0.,0.,0.));
#28500=CARTESIAN_POINT('Origin',(0.0115261780187742,-0.008,-0.00643329000430777));
#28501=CARTESIAN_POINT('',(0.011643864330556,-0.008,-0.00621272270841102));
#28502=CARTESIAN_POINT('',(0.0117444768448874,-0.008,-0.00655513261802572));
#28503=CARTESIAN_POINT('Origin',(0.0115261780187842,-0.00799999999999,-0.00643329000431777));
#28504=CARTESIAN_POINT('',(0.0117444768448874,-0.024,-0.00655513261802572));
#28505=CARTESIAN_POINT('',(0.0117444768448974,-0.00799999999999,-0.00655513261803572));
#28506=CARTESIAN_POINT('',(0.011643864330556,-0.024,-0.00621272270841102));
#28507=CARTESIAN_POINT('Origin',(0.0115261780187842,-0.02400000000001,-0.00643329000431777));
#28508=CARTESIAN_POINT('',(0.011643864330566,-0.00799999999999,-0.00621272270842102));
#28509=CARTESIAN_POINT('Origin',(-4.44089209850063E-17,-0.008,6.72997231505748E-33));
#28510=CARTESIAN_POINT('',(0.0115491497948299,-0.008,-0.00689344899281771));
#28511=CARTESIAN_POINT('Origin',(-4.44089209850063E-17,-0.00799999999999,
6.72997231505748E-33));
#28512=CARTESIAN_POINT('',(0.0115491497948299,-0.024,-0.00689344899281771));
#28513=CARTESIAN_POINT('',(0.0115491497948398,-0.00799999999999,-0.00689344899282771));
#28514=CARTESIAN_POINT('Origin',(-4.44089209850063E-17,-0.02400000000001,
6.72997231505748E-33));
#28515=CARTESIAN_POINT('Origin',(0.0113344815830301,-0.008,-0.00676531797064638));
#28516=CARTESIAN_POINT('',(0.0112023078574304,-0.008,-0.00697752095427546));
#28517=CARTESIAN_POINT('Origin',(0.0113344815830401,-0.00799999999999,-0.00676531797065638));
#28518=CARTESIAN_POINT('',(0.0112023078574304,-0.024,-0.00697752095427546));
#28519=CARTESIAN_POINT('',(0.0112023078574404,-0.00799999999999,-0.00697752095428546));
#28520=CARTESIAN_POINT('Origin',(0.0113344815830401,-0.02400000000001,-0.00676531797065638));
#28521=CARTESIAN_POINT('Origin',(0.0110345551487124,-0.008,-0.00687303373118607));
#28522=CARTESIAN_POINT('',(0.0110345551487124,-0.008,-0.00687303373118607));
#28523=CARTESIAN_POINT('',(0.0108205542946553,-0.00799999999999,-0.00673974017575289));
#28524=CARTESIAN_POINT('',(0.0110345551487124,-0.024,-0.00687303373118607));
#28525=CARTESIAN_POINT('',(0.0110345551487224,-0.016,-0.00687303373119608));
#28526=CARTESIAN_POINT('',(0.0108205542946553,-0.02400000000001,-0.00673974017575289));
#28527=CARTESIAN_POINT('Origin',(0.0105878571202839,-0.008,-0.00788272044413949));
#28528=CARTESIAN_POINT('',(0.0107333264186156,-0.008,-0.00767940127818884));
#28529=CARTESIAN_POINT('',(0.0107883847172589,-0.008,-0.00803201439194517));
#28530=CARTESIAN_POINT('Origin',(0.0105878571202939,-0.00799999999999,-0.00788272044414949));
#28531=CARTESIAN_POINT('',(0.0107883847172589,-0.024,-0.00803201439194517));
#28532=CARTESIAN_POINT('',(0.0107883847172689,-0.00799999999999,-0.00803201439195517));
#28533=CARTESIAN_POINT('',(0.0107333264186156,-0.024,-0.00767940127818884));
#28534=CARTESIAN_POINT('Origin',(0.0105878571202939,-0.02400000000001,-0.00788272044414949));
#28535=CARTESIAN_POINT('',(0.0107333264186256,-0.00799999999999,-0.00767940127819885));
#28536=CARTESIAN_POINT('Origin',(-4.44089209850063E-17,-0.008,6.72997231505748E-33));
#28537=CARTESIAN_POINT('',(0.0105505695690249,-0.008,-0.00834194112716973));
#28538=CARTESIAN_POINT('Origin',(-4.44089209850063E-17,-0.00799999999999,
6.72997231505748E-33));
#28539=CARTESIAN_POINT('',(0.0105505695690249,-0.024,-0.00834194112716973));
#28540=CARTESIAN_POINT('',(0.0105505695690349,-0.00799999999999,-0.00834194112717973));
#28541=CARTESIAN_POINT('Origin',(-4.44089209850063E-17,-0.02400000000001,
6.72997231505748E-33));
#28542=CARTESIAN_POINT('Origin',(0.010354462327965,-0.008,-0.00818688645937847));
#28543=CARTESIAN_POINT('',(0.0101957213194795,-0.008,-0.00838002188395165));
#28544=CARTESIAN_POINT('Origin',(0.010354462327975,-0.00799999999999,-0.00818688645938847));
#28545=CARTESIAN_POINT('',(0.0101957213194795,-0.024,-0.00838002188395165));
#28546=CARTESIAN_POINT('',(0.0101957213194895,-0.00799999999999,-0.00838002188396165));
#28547=CARTESIAN_POINT('Origin',(0.010354462327975,-0.02400000000001,-0.00818688645938847));
#28548=CARTESIAN_POINT('Origin',(0.0100430420778052,-0.008,-0.00825453244123692));
#28549=CARTESIAN_POINT('',(0.0100430420778052,-0.008,-0.00825453244123692));
#28550=CARTESIAN_POINT('',(0.00995338570524485,-0.00799999999999,-0.00818084247458021));
#28551=CARTESIAN_POINT('',(0.0100430420778052,-0.024,-0.00825453244123692));
#28552=CARTESIAN_POINT('',(0.0100430420778153,-0.016,-0.00825453244124692));
#28553=CARTESIAN_POINT('',(0.00995338570524485,-0.02400000000001,-0.00818084247458021));
#28554=CARTESIAN_POINT('Origin',(0.0094683750509568,-0.008,-0.00919727535166899));
#28555=CARTESIAN_POINT('',(0.00963913831581237,-0.008,-0.00901468316296458));
#28556=CARTESIAN_POINT('',(0.0096477003360128,-0.008,-0.00937146617272333));
#28557=CARTESIAN_POINT('Origin',(0.0094683750509668,-0.00799999999999,-0.00919727535167899));
#28558=CARTESIAN_POINT('',(0.0096477003360128,-0.024,-0.00937146617272333));
#28559=CARTESIAN_POINT('',(0.00964770033602281,-0.00799999999999,-0.00937146617273333));
#28560=CARTESIAN_POINT('',(0.00963913831581237,-0.024,-0.00901468316296458));
#28561=CARTESIAN_POINT('Origin',(0.0094683750509668,-0.02400000000001,-0.00919727535167899));
#28562=CARTESIAN_POINT('',(0.00963913831582238,-0.00799999999999,-0.00901468316297458));
#28563=CARTESIAN_POINT('Origin',(-4.44089209850063E-17,-0.008,6.72997231505748E-33));
#28564=CARTESIAN_POINT('',(0.00937146617272329,-0.008,-0.00964770033601285));
#28565=CARTESIAN_POINT('Origin',(-4.44089209850063E-17,-0.00799999999999,
6.72997231505748E-33));
#28566=CARTESIAN_POINT('',(0.00937146617272329,-0.024,-0.00964770033601285));
#28567=CARTESIAN_POINT('',(0.00937146617273328,-0.00799999999999,-0.00964770033602285));
#28568=CARTESIAN_POINT('Origin',(-4.44089209850063E-17,-0.02400000000001,
6.72997231505748E-33));
#28569=CARTESIAN_POINT('Origin',(0.00919727535166896,-0.008,-0.00946837505095685));
#28570=CARTESIAN_POINT('',(0.00901468316296453,-0.008,-0.00963913831581242));
#28571=CARTESIAN_POINT('Origin',(0.00919727535167896,-0.00799999999999,
-0.00946837505096685));
#28572=CARTESIAN_POINT('',(0.00901468316296453,-0.024,-0.00963913831581242));
#28573=CARTESIAN_POINT('',(0.00901468316297454,-0.00799999999999,-0.00963913831582242));
#28574=CARTESIAN_POINT('Origin',(0.00919727535167896,-0.02400000000001,
-0.00946837505096685));
#28575=CARTESIAN_POINT('Origin',(0.00887968977248941,-0.008,-0.00949479381262943));
#28576=CARTESIAN_POINT('',(0.00887968977248941,-0.008,-0.00949479381262943));
#28577=CARTESIAN_POINT('',(0.00881874742507023,-0.00799999999999,-0.00942962993438205));
#28578=CARTESIAN_POINT('',(0.00887968977248941,-0.024,-0.00949479381262943));
#28579=CARTESIAN_POINT('',(0.00887968977249942,-0.016,-0.00949479381263943));
#28580=CARTESIAN_POINT('',(0.00881874742507023,-0.02400000000001,-0.00942962993438205));
#28581=CARTESIAN_POINT('Origin',(0.00818688645937843,-0.008,-0.010354462327965));
#28582=CARTESIAN_POINT('',(0.0083800218839516,-0.008,-0.0101957213194796));
#28583=CARTESIAN_POINT('',(0.00834194112716969,-0.008,-0.0105505695690249));
#28584=CARTESIAN_POINT('Origin',(0.00818688645938842,-0.00799999999999,
-0.010354462327975));
#28585=CARTESIAN_POINT('',(0.00834194112716969,-0.024,-0.0105505695690249));
#28586=CARTESIAN_POINT('',(0.00834194112717969,-0.00799999999999,-0.0105505695690349));
#28587=CARTESIAN_POINT('',(0.0083800218839516,-0.024,-0.0101957213194796));
#28588=CARTESIAN_POINT('Origin',(0.00818688645938842,-0.02400000000001,
-0.010354462327975));
#28589=CARTESIAN_POINT('',(0.00838002188396161,-0.00799999999999,-0.0101957213194896));
#28590=CARTESIAN_POINT('Origin',(-4.44089209850063E-17,-0.008,6.72997231505748E-33));
#28591=CARTESIAN_POINT('',(0.00803201439194512,-0.008,-0.0107883847172589));
#28592=CARTESIAN_POINT('Origin',(-4.44089209850063E-17,-0.00799999999999,
6.72997231505748E-33));
#28593=CARTESIAN_POINT('',(0.00803201439194512,-0.024,-0.0107883847172589));
#28594=CARTESIAN_POINT('',(0.00803201439195512,-0.00799999999999,-0.0107883847172689));
#28595=CARTESIAN_POINT('Origin',(-4.44089209850063E-17,-0.02400000000001,
6.72997231505748E-33));
#28596=CARTESIAN_POINT('Origin',(0.00788272044413945,-0.008,-0.0105878571202839));
#28597=CARTESIAN_POINT('',(0.00767940127818881,-0.008,-0.0107333264186156));
#28598=CARTESIAN_POINT('Origin',(0.00788272044414944,-0.00799999999999,
-0.0105878571202939));
#28599=CARTESIAN_POINT('',(0.00767940127818881,-0.024,-0.0107333264186156));
#28600=CARTESIAN_POINT('',(0.00767940127819881,-0.00799999999999,-0.0107333264186256));
#28601=CARTESIAN_POINT('Origin',(0.00788272044414944,-0.02400000000001,
-0.0105878571202939));
#28602=CARTESIAN_POINT('Origin',(0.00756440351325119,-0.008,-0.0105725966294337));
#28603=CARTESIAN_POINT('',(0.00756440351325119,-0.008,-0.0105725966294337));
#28604=CARTESIAN_POINT('',(0.00746427554955173,-0.00799999999999,-0.0104326500269426));
#28605=CARTESIAN_POINT('',(0.00756440351325119,-0.024,-0.0105725966294337));
#28606=CARTESIAN_POINT('',(0.00756440351326119,-0.016,-0.0105725966294437));
#28607=CARTESIAN_POINT('',(0.00746427554955173,-0.02400000000001,-0.0104326500269426));
#28608=CARTESIAN_POINT('Origin',(0.00676531797064634,-0.008,-0.0113344815830301));
#28609=CARTESIAN_POINT('',(0.00697752095427543,-0.008,-0.0112023078574304));
#28610=CARTESIAN_POINT('',(0.00689344899281767,-0.008,-0.0115491497948299));
#28611=CARTESIAN_POINT('Origin',(0.00676531797065634,-0.00799999999999,
-0.0113344815830401));
#28612=CARTESIAN_POINT('',(0.00689344899281767,-0.024,-0.0115491497948299));
#28613=CARTESIAN_POINT('',(0.00689344899282767,-0.00799999999999,-0.0115491497948399));
#28614=CARTESIAN_POINT('',(0.00697752095427543,-0.024,-0.0112023078574304));
#28615=CARTESIAN_POINT('Origin',(0.00676531797065634,-0.02400000000001,
-0.0113344815830401));
#28616=CARTESIAN_POINT('',(0.00697752095428543,-0.00799999999999,-0.0112023078574404));
#28617=CARTESIAN_POINT('Origin',(-4.44089209850063E-17,-0.008,6.72997231505748E-33));
#28618=CARTESIAN_POINT('',(0.00655513261802568,-0.008,-0.0117444768448874));
#28619=CARTESIAN_POINT('Origin',(-4.44089209850063E-17,-0.00799999999999,
6.72997231505748E-33));
#28620=CARTESIAN_POINT('',(0.00655513261802568,-0.024,-0.0117444768448874));
#28621=CARTESIAN_POINT('',(0.00655513261803568,-0.00799999999999,-0.0117444768448974));
#28622=CARTESIAN_POINT('Origin',(-4.44089209850063E-17,-0.02400000000001,
6.72997231505748E-33));
#28623=CARTESIAN_POINT('Origin',(0.00643329000430773,-0.008,-0.0115261780187742));
#28624=CARTESIAN_POINT('',(0.00621272270841099,-0.008,-0.011643864330556));
#28625=CARTESIAN_POINT('Origin',(0.00643329000431773,-0.00799999999999,
-0.0115261780187842));
#28626=CARTESIAN_POINT('',(0.00621272270841099,-0.024,-0.011643864330556));
#28627=CARTESIAN_POINT('',(0.00621272270842099,-0.00799999999999,-0.011643864330566));
#28628=CARTESIAN_POINT('Origin',(0.00643329000431773,-0.02400000000001,
-0.0115261780187842));
#28629=CARTESIAN_POINT('Origin',(0.00611968821265236,-0.008,-0.0114694993866308));
#28630=CARTESIAN_POINT('',(0.00611968821265236,-0.008,-0.0114694993866308));
#28631=CARTESIAN_POINT('',(0.00594871026243935,-0.00799999999999,-0.0111490530784194));
#28632=CARTESIAN_POINT('',(0.00611968821265236,-0.024,-0.0114694993866308));
#28633=CARTESIAN_POINT('',(0.00611968821266236,-0.016,-0.0114694993866408));
#28634=CARTESIAN_POINT('',(0.00594871026243935,-0.02400000000001,-0.0111490530784194));
#28635=CARTESIAN_POINT('Origin',(0.00711094643726556,-0.008,-0.0114165205192449));
#28636=CARTESIAN_POINT('',(0.00687303373118604,-0.024,-0.0110345551487125));
#28637=CARTESIAN_POINT('',(0.00685869652879261,-0.02400000000001,-0.0110115369799216));
#28638=CARTESIAN_POINT('',(0.00687303373118604,-0.008,-0.0110345551487125));
#28639=CARTESIAN_POINT('',(0.00687303373119604,-0.016,-0.0110345551487225));
#28640=CARTESIAN_POINT('',(0.00685869652879261,-0.00799999999999,-0.0110115369799216));
#28641=CARTESIAN_POINT('Origin',(0.00854026625651046,-0.008,-0.010390685842037));
#28642=CARTESIAN_POINT('',(0.00825453244123687,-0.024,-0.0100430420778053));
#28643=CARTESIAN_POINT('',(0.00832370938221696,-0.02400000000001,-0.0101272075873608));
#28644=CARTESIAN_POINT('',(0.00825453244123687,-0.008,-0.0100430420778053));
#28645=CARTESIAN_POINT('',(0.00825453244124687,-0.016,-0.0100430420778153));
#28646=CARTESIAN_POINT('',(0.00832370938221696,-0.00799999999999,-0.0101272075873608));
#28647=CARTESIAN_POINT('Origin',(0.0109385711281449,-0.008,-0.00782624825024839));
#28648=CARTESIAN_POINT('',(0.0105725966294337,-0.024,-0.00756440351325123));
#28649=CARTESIAN_POINT('',(0.0106156372762982,-0.02400000000001,-0.00759519791805035));
#28650=CARTESIAN_POINT('',(0.0105725966294337,-0.008,-0.00756440351325123));
#28651=CARTESIAN_POINT('',(0.0105725966294436,-0.016,-0.00756440351326123));
#28652=CARTESIAN_POINT('',(0.0106156372762982,-0.00799999999999,-0.00759519791805035));
#28653=CARTESIAN_POINT('Origin',(0.0118665205192449,-0.008,-0.0063315235738596));
#28654=CARTESIAN_POINT('',(0.0114694993866308,-0.024,-0.0061196882126524));
#28655=CARTESIAN_POINT('',(0.0113475636447265,-0.02400000000001,-0.00605462794304299));
#28656=CARTESIAN_POINT('',(0.0114694993866308,-0.008,-0.0061196882126524));
#28657=CARTESIAN_POINT('',(0.0114694993866408,-0.016,-0.0061196882126624));
#28658=CARTESIAN_POINT('',(0.0113475636447265,-0.00799999999999,-0.00605462794304299));
#28659=CARTESIAN_POINT('Origin',(-4.44089209850063E-17,-0.016,6.72997231505748E-33));
#28660=CARTESIAN_POINT('',(0.0055966442585078,-0.008,-0.0117336086965482));
#28661=CARTESIAN_POINT('Origin',(-4.44089209850063E-17,-0.00799999999999,
6.72997231505748E-33));
#28662=CARTESIAN_POINT('',(0.0055966442585078,-0.024,-0.0117336086965482));
#28663=CARTESIAN_POINT('',(0.0055966442585178,-0.016,-0.0117336086965582));
#28664=CARTESIAN_POINT('Origin',(-4.44089209850063E-17,-0.02400000000001,
6.72997231505748E-33));
#28665=CARTESIAN_POINT('Origin',(-4.44089209850063E-17,-0.016,6.72997231505748E-33));
#28666=CARTESIAN_POINT('Origin',(-4.44089209850063E-17,-0.02400000000001,
6.72997231505748E-33));
#28667=CARTESIAN_POINT('Origin',(-4.44089209850063E-17,-0.00799999999999,
6.72997231505748E-33));
#28668=CARTESIAN_POINT('Origin',(0.00907128985548541,-0.024,-0.00907128985548545));
#28669=CARTESIAN_POINT('',(0.00598410424563526,-0.024,-0.0125459354524631));
#28670=CARTESIAN_POINT('',(0.00598410424564526,-0.02400000000001,-0.0125459354524731));
#28671=CARTESIAN_POINT('',(0.0125459354524631,-0.024,-0.0059841042456353));
#28672=CARTESIAN_POINT('Origin',(-4.44089209850063E-17,-0.02400000000001,
6.72997231505748E-33));
#28673=CARTESIAN_POINT('',(0.0117336086965482,-0.024,-0.00559664425850784));
#28674=CARTESIAN_POINT('',(0.0117336086965582,-0.02400000000001,-0.00559664425851784));
#28675=CARTESIAN_POINT('Origin',(-4.44089209850063E-17,-0.02400000000001,
6.72997231505748E-33));
#28676=CARTESIAN_POINT('Origin',(-4.44089209850063E-17,-0.02400000000001,
6.72997231505748E-33));
#28677=CARTESIAN_POINT('',(0.00949479381262939,-0.024,-0.00887968977248946));
#28678=CARTESIAN_POINT('Origin',(-4.44089209850063E-17,-0.02400000000001,
6.72997231505748E-33));
#28679=CARTESIAN_POINT('',(0.00959396290421598,-0.02400000000001,-0.00897243436344028));
#28680=CARTESIAN_POINT('Origin',(-4.44089209850063E-17,-0.02400000000001,
6.72997231505748E-33));
#28681=CARTESIAN_POINT('Origin',(-4.44089209850063E-17,-0.016,6.72997231505748E-33));
#28682=CARTESIAN_POINT('',(0.00949479381262939,-0.008,-0.00887968977248946));
#28683=CARTESIAN_POINT('Origin',(-4.44089209850063E-17,-0.00799999999999,
6.72997231505748E-33));
#28684=CARTESIAN_POINT('',(0.00949479381263939,-0.016,-0.00887968977249946));
#28685=CARTESIAN_POINT('Origin',(-4.44089209850063E-17,-0.016,6.72997231505748E-33));
#28686=CARTESIAN_POINT('',(0.0117336086965482,-0.008,-0.00559664425850784));
#28687=CARTESIAN_POINT('',(0.0117336086965582,-0.016,-0.00559664425851784));
#28688=CARTESIAN_POINT('Origin',(-4.44089209850063E-17,-0.00799999999999,
6.72997231505748E-33));
#28689=CARTESIAN_POINT('Origin',(0.00982345975229732,-0.008,-0.00918706364922948));
#28690=CARTESIAN_POINT('',(0.00959396290421598,-0.00799999999999,-0.00897243436344028));
#28691=CARTESIAN_POINT('Origin',(-4.44089209850063E-17,-0.016,6.72997231505748E-33));
#28692=CARTESIAN_POINT('Origin',(-4.44089209850063E-17,-0.00799999999999,
6.72997231505748E-33));
#28693=CARTESIAN_POINT('Origin',(-4.44089209850063E-17,-0.016,6.72997231505748E-33));
#28694=CARTESIAN_POINT('',(0.00598410424563526,-0.008,-0.0125459354524631));
#28695=CARTESIAN_POINT('',(0.00598410424564526,-0.016,-0.0125459354524731));
#28696=CARTESIAN_POINT('',(0.0125459354524631,-0.008,-0.0059841042456353));
#28697=CARTESIAN_POINT('Origin',(-4.44089209850063E-17,-0.00799999999999,
6.72997231505748E-33));
#28698=CARTESIAN_POINT('',(0.0125459354524731,-0.016,-0.0059841042456453));
#28699=CARTESIAN_POINT('Origin',(0.0117336086965482,-0.016,-0.00559664425850784));
#28700=CARTESIAN_POINT('',(0.0117336086965582,-0.00799999999999,-0.00559664425851784));
#28701=CARTESIAN_POINT('Origin',(-4.44089209850063E-17,-0.016,6.72997231505748E-33));
#28702=CARTESIAN_POINT('Origin',(-4.44089209850063E-17,-0.00799999999999,
6.72997231505748E-33));
#28703=CARTESIAN_POINT('Origin',(0.00598410424563526,-0.016,-0.0125459354524631));
#28704=CARTESIAN_POINT('',(0.00598410424564526,-0.00799999999999,-0.0125459354524731));
#28705=CARTESIAN_POINT('Origin',(0.00907128985548541,-0.008,-0.00907128985548545));
#28706=CARTESIAN_POINT('',(0.,0.,0.));
#28707=CARTESIAN_POINT('Origin',(-4.36800060759181E-17,-0.02565,1.40756589985541E-33));
#28708=CARTESIAN_POINT('',(0.00449993154767073,-0.02565000000001,-2.48206824506692E-5));
#28709=CARTESIAN_POINT('Origin',(-4.3680006075916E-17,-0.02565000000001,
1.40756589985638E-33));
#28710=CARTESIAN_POINT('',(-0.00249996197092825,-0.02565000000001,1.37892680281496E-5));
#28711=CARTESIAN_POINT('Origin',(-4.3680006075916E-17,-0.02565000000001,
1.40756589985638E-33));
#28712=CARTESIAN_POINT('Origin',(-4.39914640946565E-17,-0.02415,1.26341004351803E-33));
#28713=CARTESIAN_POINT('',(-0.00249996197092825,-0.02264999999999,1.37892680281496E-5));
#28714=CARTESIAN_POINT('',(-0.00249996197092825,-0.02415,1.37892680281496E-5));
#28715=CARTESIAN_POINT('Origin',(-4.4302922113397E-17,-0.02264999999999,
1.11925418717968E-33));
#28716=CARTESIAN_POINT('Origin',(-4.39914640946565E-17,-0.02415,1.26341004351803E-33));
#28717=CARTESIAN_POINT('',(0.00449993154767073,-0.02264999999999,-2.48206824506692E-5));
#28718=CARTESIAN_POINT('Origin',(-4.4302922113397E-17,-0.02264999999999,
1.11925418717968E-33));
#28719=CARTESIAN_POINT('',(0.00449993154767073,-0.02415,-2.48206824506692E-5));
#28720=CARTESIAN_POINT('Origin',(-4.43029221133949E-17,-0.02265,1.11925418718065E-33));
#28721=CARTESIAN_POINT('',(0.,0.,0.));
#28722=CARTESIAN_POINT('Origin',(-4.56515315114362E-17,-0.00365,-6.77116287837691E-17));
#28723=CARTESIAN_POINT('',(0.0116511274118543,-0.02925,-0.00888108833605083));
#28724=CARTESIAN_POINT('',(0.0132228744157255,-0.02475,-0.0063069875682416));
#28725=CARTESIAN_POINT('Origin',(-4.56515315114362E-17,-0.02475000000001,
-6.77116287837691E-17));
#28726=CARTESIAN_POINT('',(0.00888108833605071,-0.02925,-0.0116511274118544));
#28727=CARTESIAN_POINT('Origin',(-4.56515315114362E-17,-0.02925000000001,
-6.77116287837691E-17));
#28728=CARTESIAN_POINT('',(0.00630698756824148,-0.02475,-0.0132228744157256));
#28729=CARTESIAN_POINT('Origin',(-4.56515315114362E-17,-0.02475000000001,
-6.77116287837691E-17));
#28730=CARTESIAN_POINT('',(0.00630698756824148,-0.00815,-0.0132228744157256));
#28731=CARTESIAN_POINT('',(0.00630698756825148,-0.00364999999999,-0.0132228744157356));
#28732=CARTESIAN_POINT('',(0.00888108833605071,-0.00365,-0.0116511274118544));
#28733=CARTESIAN_POINT('Origin',(-4.56515315114362E-17,-0.00814999999999,
-6.77116287837691E-17));
#28734=CARTESIAN_POINT('',(0.0116511274118543,-0.00365,-0.00888108833605083));
#28735=CARTESIAN_POINT('Origin',(-4.56515315114362E-17,-0.00364999999999,
-6.77116287837691E-17));
#28736=CARTESIAN_POINT('',(0.0132228744157255,-0.00815,-0.0063069875682416));
#28737=CARTESIAN_POINT('Origin',(-4.56515315114362E-17,-0.00814999999999,
-6.77116287837691E-17));
#28738=CARTESIAN_POINT('',(0.0132228744157355,-0.00364999999999,-0.0063069875682516));
#28739=CARTESIAN_POINT('',(0.0113653314426162,-0.02325,-0.0092440110990566));
#28740=CARTESIAN_POINT('',(0.0113653314426162,-0.00965,-0.0092440110990566));
#28741=CARTESIAN_POINT('',(0.0113653314426262,-0.00364999999999,-0.0092440110990666));
#28742=CARTESIAN_POINT('',(0.00924401109905649,-0.00965,-0.0113653314426163));
#28743=CARTESIAN_POINT('Ctrl Pts',(0.0113653314426161,-0.00965,-0.00924401109905659));
#28744=CARTESIAN_POINT('Ctrl Pts',(0.0113653314426161,-0.00946151448459537,
-0.00924401109905659));
#28745=CARTESIAN_POINT('Ctrl Pts',(0.0113415286147626,-0.00926055630226628,
-0.00927351838063712));
#28746=CARTESIAN_POINT('Ctrl Pts',(0.0112435430943065,-0.00889102670991339,
-0.00939207927644872));
#28747=CARTESIAN_POINT('Ctrl Pts',(0.011169215384428,-0.00872244398548004,
-0.00948097768002299));
#28748=CARTESIAN_POINT('Ctrl Pts',(0.010994642278187,-0.00845623616911263,
-0.00968287927809851));
#28749=CARTESIAN_POINT('Ctrl Pts',(0.0108827047851676,-0.00834081748849188,
-0.00980935406895069));
#28750=CARTESIAN_POINT('Ctrl Pts',(0.010631656844134,-0.00818769575944871,
-0.0100809009239758));
#28751=CARTESIAN_POINT('Ctrl Pts',(0.0104923932316728,-0.00815,-0.010225835457093));
#28752=CARTESIAN_POINT('Ctrl Pts',(0.0102258354570929,-0.00815,-0.0104923932316729));
#28753=CARTESIAN_POINT('Ctrl Pts',(0.0100809009239757,-0.00818769575944871,
-0.0106316568441341));
#28754=CARTESIAN_POINT('Ctrl Pts',(0.00980935406895059,-0.00834081748849188,
-0.0108827047851677));
#28755=CARTESIAN_POINT('Ctrl Pts',(0.00968287927809842,-0.00845623616911263,
-0.0109946422781871));
#28756=CARTESIAN_POINT('Ctrl Pts',(0.0094809776800229,-0.00872244398548004,
-0.0111692153844281));
#28757=CARTESIAN_POINT('Ctrl Pts',(0.00939207927644862,-0.00889102670991339,
-0.0112435430943066));
#28758=CARTESIAN_POINT('Ctrl Pts',(0.00927351838063703,-0.00926055630226629,
-0.0113415286147627));
#28759=CARTESIAN_POINT('Ctrl Pts',(0.00924401109905649,-0.00946151448459537,
-0.0113653314426162));
#28760=CARTESIAN_POINT('Ctrl Pts',(0.00924401109905649,-0.00965,-0.0113653314426162));
#28761=CARTESIAN_POINT('',(0.00924401109905649,-0.02325,-0.0113653314426163));
#28762=CARTESIAN_POINT('',(0.00924401109906649,-0.00364999999999,-0.0113653314426263));
#28763=CARTESIAN_POINT('Ctrl Pts',(0.00924401109905649,-0.02325,-0.0113653314426162));
#28764=CARTESIAN_POINT('Ctrl Pts',(0.00924401109905649,-0.0234384855154046,
-0.0113653314426162));
#28765=CARTESIAN_POINT('Ctrl Pts',(0.00927351838063703,-0.0236394436977337,
-0.0113415286147627));
#28766=CARTESIAN_POINT('Ctrl Pts',(0.00939207927644862,-0.0240089732900866,
-0.0112435430943066));
#28767=CARTESIAN_POINT('Ctrl Pts',(0.0094809776800229,-0.02417755601452,
-0.0111692153844281));
#28768=CARTESIAN_POINT('Ctrl Pts',(0.00968287927809842,-0.0244437638308874,
-0.0109946422781871));
#28769=CARTESIAN_POINT('Ctrl Pts',(0.00980935406895059,-0.0245591825115081,
-0.0108827047851677));
#28770=CARTESIAN_POINT('Ctrl Pts',(0.0100809009239757,-0.0247123042405513,
-0.0106316568441341));
#28771=CARTESIAN_POINT('Ctrl Pts',(0.0102258354570929,-0.02475,-0.0104923932316729));
#28772=CARTESIAN_POINT('Ctrl Pts',(0.0104923932316728,-0.02475,-0.010225835457093));
#28773=CARTESIAN_POINT('Ctrl Pts',(0.010631656844134,-0.0247123042405513,
-0.0100809009239758));
#28774=CARTESIAN_POINT('Ctrl Pts',(0.0108827047851676,-0.0245591825115081,
-0.00980935406895069));
#28775=CARTESIAN_POINT('Ctrl Pts',(0.010994642278187,-0.0244437638308874,
-0.00968287927809851));
#28776=CARTESIAN_POINT('Ctrl Pts',(0.011169215384428,-0.02417755601452,
-0.00948097768002299));
#28777=CARTESIAN_POINT('Ctrl Pts',(0.0112435430943065,-0.0240089732900866,
-0.00939207927644872));
#28778=CARTESIAN_POINT('Ctrl Pts',(0.0113415286147626,-0.0236394436977337,
-0.00927351838063713));
#28779=CARTESIAN_POINT('Ctrl Pts',(0.0113653314426161,-0.0234384855154046,
-0.00924401109905659));
#28780=CARTESIAN_POINT('Ctrl Pts',(0.0113653314426161,-0.02325,-0.00924401109905659));
#28781=CARTESIAN_POINT('Origin',(0.0125459354524631,-0.00365,-0.00598410424563538));
#28782=CARTESIAN_POINT('',(0.0125459354524631,-0.02475,-0.00598410424563538));
#28783=CARTESIAN_POINT('',(0.00627296772624148,-0.02475000000001,-0.00299205212282772));
#28784=CARTESIAN_POINT('',(0.0125459354524631,-0.00815,-0.00598410424563538));
#28785=CARTESIAN_POINT('',(0.00627296772624148,-0.00814999999999,-0.00299205212282772));
#28786=CARTESIAN_POINT('',(0.0125459354524731,-0.00364999999999,-0.00598410424564538));
#28787=CARTESIAN_POINT('Origin',(0.00562720108101904,-0.0059,-0.00434593004934251));
#28788=CARTESIAN_POINT('',(0.0109587138343332,-0.00365,-0.00855082400106528));
#28789=CARTESIAN_POINT('',(0.00498143443581659,-0.00364999999999,-0.0056998079758773));
#28790=CARTESIAN_POINT('Origin',(-4.56515315114362E-17,-0.00814999999999,
-6.77116287837691E-17));
#28791=CARTESIAN_POINT('Origin',(-4.56515315114362E-17,-0.00365,-6.77116287837691E-17));
#28792=CARTESIAN_POINT('',(0.00855082400106516,-0.00365,-0.0109587138343334));
#28793=CARTESIAN_POINT('',(0.00586124963718029,-0.00364999999999,-0.00531990391744792));
#28794=CARTESIAN_POINT('Origin',(-4.56515315114362E-17,-0.00364999999999,
-6.77116287837691E-17));
#28795=CARTESIAN_POINT('Origin',(0.0045073717106455,-0.0059,-0.00596567056265036));
#28796=CARTESIAN_POINT('',(0.00598410424563526,-0.00815,-0.0125459354524632));
#28797=CARTESIAN_POINT('Origin',(-4.56515315114362E-17,-0.00814999999999,
-6.77116287837691E-17));
#28798=CARTESIAN_POINT('',(0.00315349378413072,-0.00814999999999,-0.0066114372078728));
#28799=CARTESIAN_POINT('Origin',(0.00630698756824148,-0.00365,-0.0132228744157256));
#28800=CARTESIAN_POINT('',(0.00598410424563526,-0.02475,-0.0125459354524632));
#28801=CARTESIAN_POINT('',(0.00315349378413072,-0.02475000000001,-0.0066114372078728));
#28802=CARTESIAN_POINT('',(0.00598410424564526,-0.00364999999999,-0.0125459354524732));
#28803=CARTESIAN_POINT('Origin',(0.0045073717106455,-0.027,-0.00596567056265036));
#28804=CARTESIAN_POINT('',(0.00855082400106516,-0.02925,-0.0109587138343334));
#28805=CARTESIAN_POINT('',(0.00586124963718029,-0.02925000000001,-0.00531990391744792));
#28806=CARTESIAN_POINT('Origin',(-4.56515315114362E-17,-0.02475000000001,
-6.77116287837691E-17));
#28807=CARTESIAN_POINT('Origin',(-4.56515315114362E-17,-0.00365,-6.77116287837691E-17));
#28808=CARTESIAN_POINT('',(0.0109587138343332,-0.02925,-0.00855082400106528));
#28809=CARTESIAN_POINT('Origin',(-4.56515315114362E-17,-0.02475000000001,
-6.77116287837691E-17));
#28810=CARTESIAN_POINT('Origin',(-4.56515315114362E-17,-0.02925000000001,
-6.77116287837691E-17));
#28811=CARTESIAN_POINT('Origin',(-4.56515315114362E-17,-0.02925,-6.77116287837691E-17));
#28812=CARTESIAN_POINT('',(0.00498143443581659,-0.02925000000001,-0.0056998079758773));
#28813=CARTESIAN_POINT('Origin',(0.00562720108101904,-0.027,-0.00434593004934251));
#28814=CARTESIAN_POINT('Origin',(0.0119501046020527,-0.00965,-0.0140714249456124));
#28815=CARTESIAN_POINT('',(0.0119501046020527,-0.00965,-0.0140714249456124));
#28816=CARTESIAN_POINT('',(0.0119501046020627,-0.00964999999999,-0.0140714249456224));
#28817=CARTESIAN_POINT('',(0.0119501046020527,-0.02325,-0.0140714249456124));
#28818=CARTESIAN_POINT('',(0.0119501046020627,-0.00964999999999,-0.0140714249456224));
#28819=CARTESIAN_POINT('',(0.0119501046020627,-0.02325000000001,-0.0140714249456224));
#28820=CARTESIAN_POINT('Origin',(0.0130107647738325,-0.00965,-0.0130107647738326));
#28821=CARTESIAN_POINT('',(0.0140714249456123,-0.00965,-0.0119501046020528));
#28822=CARTESIAN_POINT('',(0.0140714249456223,-0.00964999999999,-0.0119501046020628));
#28823=CARTESIAN_POINT('Origin',(0.0130107647738425,-0.00964999999999,-0.0130107647738426));
#28824=CARTESIAN_POINT('Origin',(0.0130107647738325,-0.02325,-0.0130107647738326));
#28825=CARTESIAN_POINT('',(0.0140714249456123,-0.02325,-0.0119501046020528));
#28826=CARTESIAN_POINT('Origin',(0.0130107647738425,-0.02325000000001,-0.0130107647738426));
#28827=CARTESIAN_POINT('',(0.0140714249456223,-0.02325000000001,-0.0119501046020628));
#28828=CARTESIAN_POINT('Origin',(0.0140714249456123,-0.02325,-0.0119501046020528));
#28829=CARTESIAN_POINT('',(0.0140714249456223,-0.02325000000001,-0.0119501046020628));
#28830=CARTESIAN_POINT('Origin',(-4.56515315114362E-17,-0.00365,-6.77116287837691E-17));
#28831=CARTESIAN_POINT('',(0.00195871341465237,-0.02925,-0.014518468988129));
#28832=CARTESIAN_POINT('',(0.00489027048777469,-0.02475,-0.0138096978445005));
#28833=CARTESIAN_POINT('Origin',(-4.56515315114362E-17,-0.02475000000001,
-6.77116287837691E-17));
#28834=CARTESIAN_POINT('',(-0.00195871341465248,-0.02925,-0.014518468988129));
#28835=CARTESIAN_POINT('Origin',(-4.56515315114362E-17,-0.02925000000001,
-6.77116287837691E-17));
#28836=CARTESIAN_POINT('',(-0.0048902704877748,-0.02475,-0.0138096978445005));
#28837=CARTESIAN_POINT('Origin',(-4.56515315114362E-17,-0.02475000000001,
-6.77116287837691E-17));
#28838=CARTESIAN_POINT('',(-0.0048902704877748,-0.00815,-0.0138096978445005));
#28839=CARTESIAN_POINT('',(-0.0048902704877848,-0.00364999999999,-0.0138096978445105));
#28840=CARTESIAN_POINT('',(-0.00195871341465248,-0.00365,-0.014518468988129));
#28841=CARTESIAN_POINT('Origin',(-4.56515315114362E-17,-0.00814999999999,
-6.77116287837691E-17));
#28842=CARTESIAN_POINT('',(0.00195871341465237,-0.00365,-0.014518468988129));
#28843=CARTESIAN_POINT('Origin',(-4.56515315114362E-17,-0.00364999999999,
-6.77116287837691E-17));
#28844=CARTESIAN_POINT('',(0.00489027048777469,-0.00815,-0.0138096978445005));
#28845=CARTESIAN_POINT('Origin',(-4.56515315114362E-17,-0.00814999999999,
-6.77116287837691E-17));
#28846=CARTESIAN_POINT('',(0.00489027048778469,-0.00364999999999,-0.0138096978445105));
#28847=CARTESIAN_POINT('',(0.00149999999999995,-0.02325,-0.0145730058670133));
#28848=CARTESIAN_POINT('',(0.00149999999999995,-0.00965,-0.0145730058670133));
#28849=CARTESIAN_POINT('',(0.00150000000000995,-0.00364999999999,-0.0145730058670233));
#28850=CARTESIAN_POINT('',(-0.00150000000000005,-0.00965,-0.0145730058670133));
#28851=CARTESIAN_POINT('Ctrl Pts',(0.00149999999999995,-0.00965,-0.0145730058670132));
#28852=CARTESIAN_POINT('Ctrl Pts',(0.00149999999999995,-0.00946151448459537,
-0.0145730058670132));
#28853=CARTESIAN_POINT('Ctrl Pts',(0.00146230406011329,-0.00926055630226629,
-0.0145770395249265));
#28854=CARTESIAN_POINT('Ctrl Pts',(0.00130918262072881,-0.00889102670991339,
-0.0145915885123659));
#28855=CARTESIAN_POINT('Ctrl Pts',(0.00119376432903963,-0.00872244398548004,
-0.0146018915486848));
#28856=CARTESIAN_POINT('Ctrl Pts',(0.000927556512672221,-0.00845623616911263,
-0.0146212157105806));
#28857=CARTESIAN_POINT('Ctrl Pts',(0.000758973570028426,-0.00834081748849188,
-0.0146314951324582));
#28858=CARTESIAN_POINT('Ctrl Pts',(0.000389443245922543,-0.00818769575944871,
-0.0146459900535486));
#28859=CARTESIAN_POINT('Ctrl Pts',(0.000188484809983391,-0.00815,-0.0146500000000001));
#28860=CARTESIAN_POINT('Ctrl Pts',(-0.000188484809983482,-0.00815,-0.0146500000000001));
#28861=CARTESIAN_POINT('Ctrl Pts',(-0.000389443245922634,-0.00818769575944871,
-0.0146459900535486));
#28862=CARTESIAN_POINT('Ctrl Pts',(-0.000758973570028517,-0.00834081748849188,
-0.0146314951324582));
#28863=CARTESIAN_POINT('Ctrl Pts',(-0.000927556512672312,-0.00845623616911263,
-0.0146212157105806));
#28864=CARTESIAN_POINT('Ctrl Pts',(-0.00119376432903972,-0.00872244398548004,
-0.0146018915486848));
#28865=CARTESIAN_POINT('Ctrl Pts',(-0.0013091826207289,-0.00889102670991339,
-0.0145915885123659));
#28866=CARTESIAN_POINT('Ctrl Pts',(-0.00146230406011339,-0.00926055630226629,
-0.0145770395249265));
#28867=CARTESIAN_POINT('Ctrl Pts',(-0.00150000000000005,-0.00946151448459537,
-0.0145730058670132));
#28868=CARTESIAN_POINT('Ctrl Pts',(-0.00150000000000005,-0.00965,-0.0145730058670132));
#28869=CARTESIAN_POINT('',(-0.00150000000000005,-0.02325,-0.0145730058670133));
#28870=CARTESIAN_POINT('',(-0.00150000000001003,-0.00364999999999,-0.0145730058670233));
#28871=CARTESIAN_POINT('Ctrl Pts',(-0.00150000000000005,-0.02325,-0.0145730058670132));
#28872=CARTESIAN_POINT('Ctrl Pts',(-0.00150000000000005,-0.0234384855154046,
-0.0145730058670132));
#28873=CARTESIAN_POINT('Ctrl Pts',(-0.00146230406011339,-0.0236394436977337,
-0.0145770395249265));
#28874=CARTESIAN_POINT('Ctrl Pts',(-0.0013091826207289,-0.0240089732900866,
-0.0145915885123659));
#28875=CARTESIAN_POINT('Ctrl Pts',(-0.00119376432903972,-0.02417755601452,
-0.0146018915486848));
#28876=CARTESIAN_POINT('Ctrl Pts',(-0.000927556512672313,-0.0244437638308874,
-0.0146212157105806));
#28877=CARTESIAN_POINT('Ctrl Pts',(-0.000758973570028516,-0.0245591825115081,
-0.0146314951324582));
#28878=CARTESIAN_POINT('Ctrl Pts',(-0.000389443245922634,-0.0247123042405513,
-0.0146459900535486));
#28879=CARTESIAN_POINT('Ctrl Pts',(-0.000188484809983483,-0.02475,-0.0146500000000001));
#28880=CARTESIAN_POINT('Ctrl Pts',(0.000188484809983392,-0.02475,-0.0146500000000001));
#28881=CARTESIAN_POINT('Ctrl Pts',(0.000389443245922547,-0.0247123042405513,
-0.0146459900535486));
#28882=CARTESIAN_POINT('Ctrl Pts',(0.000758973570028428,-0.0245591825115081,
-0.0146314951324582));
#28883=CARTESIAN_POINT('Ctrl Pts',(0.000927556512672222,-0.0244437638308874,
-0.0146212157105806));
#28884=CARTESIAN_POINT('Ctrl Pts',(0.00119376432903963,-0.02417755601452,
-0.0146018915486848));
#28885=CARTESIAN_POINT('Ctrl Pts',(0.00130918262072881,-0.0240089732900866,
-0.0145915885123659));
#28886=CARTESIAN_POINT('Ctrl Pts',(0.00146230406011329,-0.0236394436977337,
-0.0145770395249265));
#28887=CARTESIAN_POINT('Ctrl Pts',(0.00149999999999995,-0.0234384855154046,
-0.0145730058670132));
#28888=CARTESIAN_POINT('Ctrl Pts',(0.00149999999999995,-0.02325,-0.0145730058670132));
#28889=CARTESIAN_POINT('Origin',(0.00463991534334936,-0.00365,-0.0131027167261814));
#28890=CARTESIAN_POINT('',(0.00463991534334936,-0.02475,-0.0131027167261814));
#28891=CARTESIAN_POINT('',(0.00231995767168467,-0.02475000000001,-0.00655135836310071));
#28892=CARTESIAN_POINT('',(0.00463991534334936,-0.00815,-0.0131027167261814));
#28893=CARTESIAN_POINT('',(0.00231995767168467,-0.00814999999999,-0.00655135836310071));
#28894=CARTESIAN_POINT('',(0.00463991534335936,-0.00364999999999,-0.0131027167261914));
#28895=CARTESIAN_POINT('Origin',(0.000905995435036393,-0.0059,-0.00705206865194137));
#28896=CARTESIAN_POINT('',(0.00170263522945395,-0.00365,-0.0137953265012259));
#28897=CARTESIAN_POINT('',(-0.000507966801611876,-0.00364999999999,-0.00755277894080202));
#28898=CARTESIAN_POINT('Origin',(-4.56515315114362E-17,-0.00814999999999,
-6.77116287837691E-17));
#28899=CARTESIAN_POINT('Origin',(-4.56515315114362E-17,-0.00365,-6.77116287837691E-17));
#28900=CARTESIAN_POINT('',(-0.00170263522945404,-0.00365,-0.0137953265012259));
#28901=CARTESIAN_POINT('',(0.000382789229399116,-0.00364999999999,-0.00790626949996159));
#28902=CARTESIAN_POINT('Origin',(-4.56515315114362E-17,-0.00364999999999,
-6.77116287837691E-17));
#28903=CARTESIAN_POINT('Origin',(-0.00103117300724916,-0.0059,-0.00740555921110094));
#28904=CARTESIAN_POINT('',(-0.00463991534334947,-0.00815,-0.0131027167261814));
#28905=CARTESIAN_POINT('Origin',(-4.56515315114362E-17,-0.00814999999999,
-6.77116287837691E-17));
#28906=CARTESIAN_POINT('',(-0.00244513524389743,-0.00814999999999,-0.00690484892226028));
#28907=CARTESIAN_POINT('Origin',(-0.0048902704877748,-0.00365,-0.0138096978445005));
#28908=CARTESIAN_POINT('',(-0.00463991534334947,-0.02475,-0.0131027167261814));
#28909=CARTESIAN_POINT('',(-0.00244513524389742,-0.02475000000001,-0.00690484892226028));
#28910=CARTESIAN_POINT('',(-0.00463991534335947,-0.00364999999999,-0.0131027167261914));
#28911=CARTESIAN_POINT('Origin',(-0.00103117300724916,-0.027,-0.00740555921110094));
#28912=CARTESIAN_POINT('',(-0.00170263522945404,-0.02925,-0.0137953265012259));
#28913=CARTESIAN_POINT('',(0.000382789229399114,-0.02925000000001,-0.00790626949996159));
#28914=CARTESIAN_POINT('Origin',(-4.56515315114362E-17,-0.02475000000001,
-6.77116287837691E-17));
#28915=CARTESIAN_POINT('Origin',(-4.56515315114362E-17,-0.00365,-6.77116287837691E-17));
#28916=CARTESIAN_POINT('',(0.00170263522945395,-0.02925,-0.0137953265012259));
#28917=CARTESIAN_POINT('Origin',(-4.56515315114362E-17,-0.02475000000001,
-6.77116287837691E-17));
#28918=CARTESIAN_POINT('Origin',(-4.56515315114362E-17,-0.02925000000001,
-6.77116287837691E-17));
#28919=CARTESIAN_POINT('Origin',(-4.56515315114362E-17,-0.02925,-6.77116287837691E-17));
#28920=CARTESIAN_POINT('',(-0.000507966801611876,-0.02925000000001,-0.00755277894080202));
#28921=CARTESIAN_POINT('Origin',(0.000905995435036393,-0.027,-0.00705206865194137));
#28922=CARTESIAN_POINT('Origin',(-0.00150000000000005,-0.00965,-0.0184));
#28923=CARTESIAN_POINT('',(-0.00150000000000005,-0.00965,-0.0184));
#28924=CARTESIAN_POINT('',(-0.00150000000001004,-0.00964999999999,-0.0184000000000101));
#28925=CARTESIAN_POINT('',(-0.00150000000000005,-0.02325,-0.0184));
#28926=CARTESIAN_POINT('',(-0.00150000000001003,-0.00964999999999,-0.0184000000000101));
#28927=CARTESIAN_POINT('',(-0.00150000000001004,-0.02325000000001,-0.0184000000000101));
#28928=CARTESIAN_POINT('Origin',(-4.56515315114362E-17,-0.00965,-0.0184));
#28929=CARTESIAN_POINT('',(0.00149999999999995,-0.00965,-0.0184));
#28930=CARTESIAN_POINT('',(0.00150000000000995,-0.00964999999999,-0.0184000000000101));
#28931=CARTESIAN_POINT('Origin',(-4.56515315114362E-17,-0.00964999999999,
-0.0184000000000101));
#28932=CARTESIAN_POINT('Origin',(-4.56515315114362E-17,-0.02325,-0.0184));
#28933=CARTESIAN_POINT('',(0.00149999999999995,-0.02325,-0.0184));
#28934=CARTESIAN_POINT('Origin',(-4.56515315114362E-17,-0.02325000000001,
-0.0184000000000101));
#28935=CARTESIAN_POINT('',(0.00150000000000995,-0.02325000000001,-0.0184000000000101));
#28936=CARTESIAN_POINT('Origin',(0.00149999999999995,-0.02325,-0.0184));
#28937=CARTESIAN_POINT('',(0.00150000000000995,-0.02325000000001,-0.0184000000000101));
#28938=CARTESIAN_POINT('Origin',(-4.56515315114362E-17,-0.00365,-6.77116287837691E-17));
#28939=CARTESIAN_POINT('',(-0.00888108833605081,-0.02925,-0.0116511274118544));
#28940=CARTESIAN_POINT('',(-0.00630698756824158,-0.02475,-0.0132228744157256));
#28941=CARTESIAN_POINT('Origin',(-4.56515315114362E-17,-0.02475000000001,
-6.77116287837691E-17));
#28942=CARTESIAN_POINT('',(-0.0116511274118543,-0.02925,-0.00888108833605082));
#28943=CARTESIAN_POINT('Origin',(-4.56515315114362E-17,-0.02925000000001,
-6.77116287837691E-17));
#28944=CARTESIAN_POINT('',(-0.0132228744157255,-0.02475,-0.00630698756824159));
#28945=CARTESIAN_POINT('Origin',(-4.56515315114362E-17,-0.02475000000001,
-6.77116287837691E-17));
#28946=CARTESIAN_POINT('',(-0.0132228744157255,-0.00815,-0.00630698756824159));
#28947=CARTESIAN_POINT('',(-0.0132228744157355,-0.00364999999999,-0.00630698756825159));
#28948=CARTESIAN_POINT('',(-0.0116511274118543,-0.00365,-0.00888108833605082));
#28949=CARTESIAN_POINT('Origin',(-4.56515315114362E-17,-0.00814999999999,
-6.77116287837691E-17));
#28950=CARTESIAN_POINT('',(-0.00888108833605081,-0.00365,-0.0116511274118544));
#28951=CARTESIAN_POINT('Origin',(-4.56515315114362E-17,-0.00364999999999,
-6.77116287837691E-17));
#28952=CARTESIAN_POINT('',(-0.00630698756824158,-0.00815,-0.0132228744157256));
#28953=CARTESIAN_POINT('Origin',(-4.56515315114362E-17,-0.00814999999999,
-6.77116287837691E-17));
#28954=CARTESIAN_POINT('',(-0.00630698756825158,-0.00364999999999,-0.0132228744157356));
#28955=CARTESIAN_POINT('',(-0.00924401109905658,-0.02325,-0.0113653314426163));
#28956=CARTESIAN_POINT('',(-0.00924401109905658,-0.00965,-0.0113653314426163));
#28957=CARTESIAN_POINT('',(-0.00924401109906658,-0.00364999999999,-0.0113653314426263));
#28958=CARTESIAN_POINT('',(-0.0113653314426162,-0.00965,-0.0092440110990566));
#28959=CARTESIAN_POINT('Ctrl Pts',(-0.00924401109905653,-0.00965,-0.0113653314426163));
#28960=CARTESIAN_POINT('Ctrl Pts',(-0.00924401109905653,-0.00946151448459537,
-0.0113653314426163));
#28961=CARTESIAN_POINT('Ctrl Pts',(-0.00927351838063707,-0.00926055630226628,
-0.0113415286147627));
#28962=CARTESIAN_POINT('Ctrl Pts',(-0.00939207927644867,-0.00889102670991339,
-0.0112435430943067));
#28963=CARTESIAN_POINT('Ctrl Pts',(-0.00948097768002294,-0.00872244398548004,
-0.0111692153844282));
#28964=CARTESIAN_POINT('Ctrl Pts',(-0.00968287927809846,-0.00845623616911263,
-0.0109946422781872));
#28965=CARTESIAN_POINT('Ctrl Pts',(-0.00980935406895063,-0.00834081748849188,
-0.0108827047851677));
#28966=CARTESIAN_POINT('Ctrl Pts',(-0.0100809009239757,-0.00818769575944871,
-0.0106316568441342));
#28967=CARTESIAN_POINT('Ctrl Pts',(-0.010225835457093,-0.00815,-0.010492393231673));
#28968=CARTESIAN_POINT('Ctrl Pts',(-0.0104923932316729,-0.00815,-0.0102258354570931));
#28969=CARTESIAN_POINT('Ctrl Pts',(-0.0106316568441341,-0.00818769575944871,
-0.0100809009239758));
#28970=CARTESIAN_POINT('Ctrl Pts',(-0.0108827047851676,-0.00834081748849188,
-0.00980935406895074));
#28971=CARTESIAN_POINT('Ctrl Pts',(-0.0109946422781871,-0.00845623616911263,
-0.00968287927809856));
#28972=CARTESIAN_POINT('Ctrl Pts',(-0.0111692153844281,-0.00872244398548004,
-0.00948097768002304));
#28973=CARTESIAN_POINT('Ctrl Pts',(-0.0112435430943066,-0.00889102670991339,
-0.00939207927644877));
#28974=CARTESIAN_POINT('Ctrl Pts',(-0.0113415286147626,-0.00926055630226628,
-0.00927351838063717));
#28975=CARTESIAN_POINT('Ctrl Pts',(-0.0113653314426162,-0.00946151448459537,
-0.00924401109905664));
#28976=CARTESIAN_POINT('Ctrl Pts',(-0.0113653314426162,-0.00965,-0.00924401109905664));
#28977=CARTESIAN_POINT('',(-0.0113653314426162,-0.02325,-0.0092440110990566));
#28978=CARTESIAN_POINT('',(-0.0113653314426262,-0.00364999999999,-0.0092440110990666));
#28979=CARTESIAN_POINT('Ctrl Pts',(-0.0113653314426162,-0.02325,-0.00924401109905664));
#28980=CARTESIAN_POINT('Ctrl Pts',(-0.0113653314426162,-0.0234384855154046,
-0.00924401109905664));
#28981=CARTESIAN_POINT('Ctrl Pts',(-0.0113415286147626,-0.0236394436977337,
-0.00927351838063718));
#28982=CARTESIAN_POINT('Ctrl Pts',(-0.0112435430943066,-0.0240089732900866,
-0.00939207927644877));
#28983=CARTESIAN_POINT('Ctrl Pts',(-0.0111692153844281,-0.02417755601452,
-0.00948097768002304));
#28984=CARTESIAN_POINT('Ctrl Pts',(-0.0109946422781871,-0.0244437638308874,
-0.00968287927809855));
#28985=CARTESIAN_POINT('Ctrl Pts',(-0.0108827047851676,-0.0245591825115081,
-0.00980935406895074));
#28986=CARTESIAN_POINT('Ctrl Pts',(-0.0106316568441341,-0.0247123042405513,
-0.0100809009239758));
#28987=CARTESIAN_POINT('Ctrl Pts',(-0.0104923932316729,-0.02475,-0.0102258354570931));
#28988=CARTESIAN_POINT('Ctrl Pts',(-0.010225835457093,-0.02475,-0.010492393231673));
#28989=CARTESIAN_POINT('Ctrl Pts',(-0.0100809009239757,-0.0247123042405513,
-0.0106316568441342));
#28990=CARTESIAN_POINT('Ctrl Pts',(-0.00980935406895064,-0.0245591825115081,
-0.0108827047851677));
#28991=CARTESIAN_POINT('Ctrl Pts',(-0.00968287927809846,-0.0244437638308874,
-0.0109946422781872));
#28992=CARTESIAN_POINT('Ctrl Pts',(-0.00948097768002294,-0.02417755601452,
-0.0111692153844282));
#28993=CARTESIAN_POINT('Ctrl Pts',(-0.00939207927644866,-0.0240089732900866,
-0.0112435430943067));
#28994=CARTESIAN_POINT('Ctrl Pts',(-0.00927351838063707,-0.0236394436977337,
-0.0113415286147627));
#28995=CARTESIAN_POINT('Ctrl Pts',(-0.00924401109905653,-0.0234384855154046,
-0.0113653314426163));
#28996=CARTESIAN_POINT('Ctrl Pts',(-0.00924401109905653,-0.02325,-0.0113653314426163));
#28997=CARTESIAN_POINT('Origin',(-0.00598410424563536,-0.00365,-0.0125459354524632));
#28998=CARTESIAN_POINT('',(-0.00598410424563536,-0.02475,-0.0125459354524632));
#28999=CARTESIAN_POINT('',(-0.0029920521228277,-0.02475000000001,-0.0062729677262416));
#29000=CARTESIAN_POINT('',(-0.00598410424563536,-0.00815,-0.0125459354524632));
#29001=CARTESIAN_POINT('',(-0.0029920521228277,-0.00814999999999,-0.0062729677262416));
#29002=CARTESIAN_POINT('',(-0.00598410424564536,-0.00364999999999,-0.0125459354524732));
#29003=CARTESIAN_POINT('Origin',(-0.00434593004934249,-0.0059,-0.00562720108101916));
#29004=CARTESIAN_POINT('',(-0.00855082400106526,-0.00365,-0.0109587138343334));
#29005=CARTESIAN_POINT('',(-0.00569980797587729,-0.00364999999999,-0.00498143443581672));
#29006=CARTESIAN_POINT('Origin',(-4.56515315114362E-17,-0.00814999999999,
-6.77116287837691E-17));
#29007=CARTESIAN_POINT('Origin',(-4.56515315114362E-17,-0.00365,-6.77116287837691E-17));
#29008=CARTESIAN_POINT('',(-0.0109587138343333,-0.00365,-0.00855082400106528));
#29009=CARTESIAN_POINT('',(-0.0053199039174479,-0.00364999999999,-0.00586124963718042));
#29010=CARTESIAN_POINT('Origin',(-4.56515315114362E-17,-0.00364999999999,
-6.77116287837691E-17));
#29011=CARTESIAN_POINT('Origin',(-0.00596567056265034,-0.0059,-0.00450737171064562));
#29012=CARTESIAN_POINT('',(-0.0125459354524631,-0.00815,-0.00598410424563537));
#29013=CARTESIAN_POINT('Origin',(-4.56515315114362E-17,-0.00814999999999,
-6.77116287837691E-17));
#29014=CARTESIAN_POINT('',(-0.00661143720787278,-0.00814999999999,-0.00315349378413083));
#29015=CARTESIAN_POINT('Origin',(-0.0132228744157255,-0.00365,-0.00630698756824159));
#29016=CARTESIAN_POINT('',(-0.0125459354524631,-0.02475,-0.00598410424563537));
#29017=CARTESIAN_POINT('',(-0.00661143720787278,-0.02475000000001,-0.00315349378413083));
#29018=CARTESIAN_POINT('',(-0.0125459354524731,-0.00364999999999,-0.00598410424564537));
#29019=CARTESIAN_POINT('Origin',(-0.00596567056265034,-0.027,-0.00450737171064562));
#29020=CARTESIAN_POINT('',(-0.0109587138343333,-0.02925,-0.00855082400106528));
#29021=CARTESIAN_POINT('',(-0.0053199039174479,-0.02925000000001,-0.00586124963718041));
#29022=CARTESIAN_POINT('Origin',(-4.56515315114362E-17,-0.02475000000001,
-6.77116287837691E-17));
#29023=CARTESIAN_POINT('Origin',(-4.56515315114362E-17,-0.00365,-6.77116287837691E-17));
#29024=CARTESIAN_POINT('',(-0.00855082400106526,-0.02925,-0.0109587138343334));
#29025=CARTESIAN_POINT('Origin',(-4.56515315114362E-17,-0.02475000000001,
-6.77116287837691E-17));
#29026=CARTESIAN_POINT('Origin',(-4.56515315114362E-17,-0.02925000000001,
-6.77116287837691E-17));
#29027=CARTESIAN_POINT('Origin',(-4.56515315114362E-17,-0.02925,-6.77116287837691E-17));
#29028=CARTESIAN_POINT('',(-0.00569980797587729,-0.02925000000001,-0.00498143443581672));
#29029=CARTESIAN_POINT('Origin',(-0.00434593004934249,-0.027,-0.00562720108101916));
#29030=CARTESIAN_POINT('Origin',(-0.0140714249456123,-0.00965,-0.0119501046020528));
#29031=CARTESIAN_POINT('',(-0.0140714249456123,-0.00965,-0.0119501046020528));
#29032=CARTESIAN_POINT('',(-0.0140714249456223,-0.00964999999999,-0.0119501046020628));
#29033=CARTESIAN_POINT('',(-0.0140714249456123,-0.02325,-0.0119501046020528));
#29034=CARTESIAN_POINT('',(-0.0140714249456223,-0.00964999999999,-0.0119501046020628));
#29035=CARTESIAN_POINT('',(-0.0140714249456223,-0.02325000000001,-0.0119501046020628));
#29036=CARTESIAN_POINT('Origin',(-0.0130107647738325,-0.00965,-0.0130107647738326));
#29037=CARTESIAN_POINT('',(-0.0119501046020527,-0.00965,-0.0140714249456124));
#29038=CARTESIAN_POINT('',(-0.0119501046020627,-0.00964999999999,-0.0140714249456224));
#29039=CARTESIAN_POINT('Origin',(-0.0130107647738425,-0.00964999999999,
-0.0130107647738426));
#29040=CARTESIAN_POINT('Origin',(-0.0130107647738325,-0.02325,-0.0130107647738326));
#29041=CARTESIAN_POINT('',(-0.0119501046020527,-0.02325,-0.0140714249456124));
#29042=CARTESIAN_POINT('Origin',(-0.0130107647738425,-0.02325000000001,
-0.0130107647738426));
#29043=CARTESIAN_POINT('',(-0.0119501046020627,-0.02325000000001,-0.0140714249456224));
#29044=CARTESIAN_POINT('Origin',(-0.0119501046020527,-0.02325,-0.0140714249456124));
#29045=CARTESIAN_POINT('',(-0.0119501046020627,-0.02325000000001,-0.0140714249456224));
#29046=CARTESIAN_POINT('Origin',(-4.56515315114362E-17,-0.00365,-6.77116287837691E-17));
#29047=CARTESIAN_POINT('',(-0.0145184689881289,-0.02925,-0.00195871341465249));
#29048=CARTESIAN_POINT('',(-0.0138096978445004,-0.02475,-0.00489027048777481));
#29049=CARTESIAN_POINT('Origin',(-4.56515315114362E-17,-0.02475000000001,
-6.77116287837691E-17));
#29050=CARTESIAN_POINT('',(-0.0145184689881289,-0.02925,0.00195871341465236));
#29051=CARTESIAN_POINT('Origin',(-4.56515315114362E-17,-0.02925000000001,
-6.77116287837691E-17));
#29052=CARTESIAN_POINT('',(-0.0138096978445004,-0.02475,0.00489027048777468));
#29053=CARTESIAN_POINT('Origin',(-4.56515315114362E-17,-0.02475000000001,
-6.77116287837691E-17));
#29054=CARTESIAN_POINT('',(-0.0138096978445004,-0.00815,0.00489027048777468));
#29055=CARTESIAN_POINT('',(-0.0138096978445104,-0.00364999999999,0.00489027048778468));
#29056=CARTESIAN_POINT('',(-0.0145184689881289,-0.00365,0.00195871341465235));
#29057=CARTESIAN_POINT('Origin',(-4.56515315114362E-17,-0.00814999999999,
-6.77116287837691E-17));
#29058=CARTESIAN_POINT('',(-0.0145184689881289,-0.00365,-0.00195871341465249));
#29059=CARTESIAN_POINT('Origin',(-4.56515315114362E-17,-0.00364999999999,
-6.77116287837691E-17));
#29060=CARTESIAN_POINT('',(-0.0138096978445004,-0.00815,-0.00489027048777481));
#29061=CARTESIAN_POINT('Origin',(-4.56515315114362E-17,-0.00814999999999,
-6.77116287837691E-17));
#29062=CARTESIAN_POINT('',(-0.0138096978445104,-0.00364999999999,-0.00489027048778481));
#29063=CARTESIAN_POINT('',(-0.0145730058670132,-0.02325,-0.00150000000000007));
#29064=CARTESIAN_POINT('',(-0.0145730058670132,-0.00965,-0.00150000000000007));
#29065=CARTESIAN_POINT('',(-0.0145730058670232,-0.00364999999999,-0.00150000000001007));
#29066=CARTESIAN_POINT('',(-0.0145730058670132,-0.00965,0.00149999999999993));
#29067=CARTESIAN_POINT('Ctrl Pts',(-0.0145730058670132,-0.00965,-0.00150000000000007));
#29068=CARTESIAN_POINT('Ctrl Pts',(-0.0145730058670132,-0.00946151448459537,
-0.00150000000000007));
#29069=CARTESIAN_POINT('Ctrl Pts',(-0.0145770395249265,-0.00926055630226629,
-0.00146230406011341));
#29070=CARTESIAN_POINT('Ctrl Pts',(-0.0145915885123659,-0.00889102670991339,
-0.00130918262072893));
#29071=CARTESIAN_POINT('Ctrl Pts',(-0.0146018915486848,-0.00872244398548004,
-0.00119376432903975));
#29072=CARTESIAN_POINT('Ctrl Pts',(-0.0146212157105805,-0.00845623616911263,
-0.000927556512672337));
#29073=CARTESIAN_POINT('Ctrl Pts',(-0.0146314951324582,-0.00834081748849188,
-0.000758973570028542));
#29074=CARTESIAN_POINT('Ctrl Pts',(-0.0146459900535486,-0.00818769575944871,
-0.000389443245922659));
#29075=CARTESIAN_POINT('Ctrl Pts',(-0.01465,-0.00815,-0.000188484809983507));
#29076=CARTESIAN_POINT('Ctrl Pts',(-0.01465,-0.00815,0.000188484809983367));
#29077=CARTESIAN_POINT('Ctrl Pts',(-0.0146459900535486,-0.00818769575944871,
0.000389443245922518));
#29078=CARTESIAN_POINT('Ctrl Pts',(-0.0146314951324582,-0.00834081748849188,
0.000758973570028401));
#29079=CARTESIAN_POINT('Ctrl Pts',(-0.0146212157105805,-0.00845623616911263,
0.000927556512672196));
#29080=CARTESIAN_POINT('Ctrl Pts',(-0.0146018915486848,-0.00872244398548004,
0.00119376432903961));
#29081=CARTESIAN_POINT('Ctrl Pts',(-0.0145915885123659,-0.00889102670991339,
0.00130918262072879));
#29082=CARTESIAN_POINT('Ctrl Pts',(-0.0145770395249265,-0.00926055630226629,
0.00146230406011327));
#29083=CARTESIAN_POINT('Ctrl Pts',(-0.0145730058670132,-0.00946151448459537,
0.00149999999999993));
#29084=CARTESIAN_POINT('Ctrl Pts',(-0.0145730058670132,-0.00965,0.00149999999999993));
#29085=CARTESIAN_POINT('',(-0.0145730058670132,-0.02325,0.00149999999999993));
#29086=CARTESIAN_POINT('',(-0.0145730058670232,-0.00364999999999,0.00150000000000993));
#29087=CARTESIAN_POINT('Ctrl Pts',(-0.0145730058670132,-0.02325,0.00149999999999993));
#29088=CARTESIAN_POINT('Ctrl Pts',(-0.0145730058670132,-0.0234384855154046,
0.00149999999999993));
#29089=CARTESIAN_POINT('Ctrl Pts',(-0.0145770395249265,-0.0236394436977337,
0.00146230406011327));
#29090=CARTESIAN_POINT('Ctrl Pts',(-0.0145915885123659,-0.0240089732900866,
0.00130918262072879));
#29091=CARTESIAN_POINT('Ctrl Pts',(-0.0146018915486848,-0.02417755601452,
0.00119376432903961));
#29092=CARTESIAN_POINT('Ctrl Pts',(-0.0146212157105805,-0.0244437638308874,
0.000927556512672197));
#29093=CARTESIAN_POINT('Ctrl Pts',(-0.0146314951324582,-0.0245591825115081,
0.0007589735700284));
#29094=CARTESIAN_POINT('Ctrl Pts',(-0.0146459900535486,-0.0247123042405513,
0.000389443245922519));
#29095=CARTESIAN_POINT('Ctrl Pts',(-0.01465,-0.02475,0.000188484809983366));
#29096=CARTESIAN_POINT('Ctrl Pts',(-0.01465,-0.02475,-0.000188484809983508));
#29097=CARTESIAN_POINT('Ctrl Pts',(-0.0146459900535486,-0.0247123042405513,
-0.000389443245922663));
#29098=CARTESIAN_POINT('Ctrl Pts',(-0.0146314951324582,-0.0245591825115081,
-0.000758973570028544));
#29099=CARTESIAN_POINT('Ctrl Pts',(-0.0146212157105805,-0.0244437638308874,
-0.000927556512672338));
#29100=CARTESIAN_POINT('Ctrl Pts',(-0.0146018915486848,-0.02417755601452,
-0.00119376432903975));
#29101=CARTESIAN_POINT('Ctrl Pts',(-0.0145915885123659,-0.0240089732900866,
-0.00130918262072893));
#29102=CARTESIAN_POINT('Ctrl Pts',(-0.0145770395249265,-0.0236394436977337,
-0.00146230406011341));
#29103=CARTESIAN_POINT('Ctrl Pts',(-0.0145730058670132,-0.0234384855154046,
-0.00150000000000007));
#29104=CARTESIAN_POINT('Ctrl Pts',(-0.0145730058670132,-0.02325,-0.00150000000000007));
#29105=CARTESIAN_POINT('Origin',(-0.0131027167261813,-0.00365,-0.00463991534334948));
#29106=CARTESIAN_POINT('',(-0.0131027167261813,-0.02475,-0.00463991534334948));
#29107=CARTESIAN_POINT('',(-0.00655135836310069,-0.02475000000001,-0.00231995767168478));
#29108=CARTESIAN_POINT('',(-0.0131027167261813,-0.00815,-0.00463991534334948));
#29109=CARTESIAN_POINT('',(-0.00655135836310069,-0.00814999999999,-0.00231995767168478));
#29110=CARTESIAN_POINT('',(-0.0131027167261913,-0.00364999999999,-0.00463991534335948));
#29111=CARTESIAN_POINT('Origin',(-0.00705206865194135,-0.0059,-0.000905995435036507));
#29112=CARTESIAN_POINT('',(-0.0137953265012258,-0.00365,-0.00170263522945406));
#29113=CARTESIAN_POINT('',(-0.007552778940802,-0.00364999999999,0.000507966801611762));
#29114=CARTESIAN_POINT('Origin',(-4.56515315114362E-17,-0.00814999999999,
-6.77116287837691E-17));
#29115=CARTESIAN_POINT('Origin',(-4.56515315114362E-17,-0.00365,-6.77116287837691E-17));
#29116=CARTESIAN_POINT('',(-0.0137953265012258,-0.00365,0.00170263522945392));
#29117=CARTESIAN_POINT('',(-0.00790626949996156,-0.00364999999999,-0.00038278922939923));
#29118=CARTESIAN_POINT('Origin',(-4.56515315114362E-17,-0.00364999999999,
-6.77116287837691E-17));
#29119=CARTESIAN_POINT('Origin',(-0.00740555921110092,-0.0059,0.00103117300724904));
#29120=CARTESIAN_POINT('',(-0.0131027167261813,-0.00815,0.00463991534334935));
#29121=CARTESIAN_POINT('Origin',(-4.56515315114362E-17,-0.00814999999999,
-6.77116287837691E-17));
#29122=CARTESIAN_POINT('',(-0.00690484892226026,-0.00814999999999,0.00244513524389732));
#29123=CARTESIAN_POINT('Origin',(-0.0138096978445004,-0.00365,0.00489027048777468));
#29124=CARTESIAN_POINT('',(-0.0131027167261813,-0.02475,0.00463991534334935));
#29125=CARTESIAN_POINT('',(-0.00690484892226026,-0.02475000000001,0.0024451352438973));
#29126=CARTESIAN_POINT('',(-0.0131027167261913,-0.00364999999999,0.00463991534335935));
#29127=CARTESIAN_POINT('Origin',(-0.00740555921110092,-0.027,0.00103117300724904));
#29128=CARTESIAN_POINT('',(-0.0137953265012258,-0.02925,0.00170263522945392));
#29129=CARTESIAN_POINT('',(-0.00790626949996156,-0.02925000000001,-0.000382789229399229));
#29130=CARTESIAN_POINT('Origin',(-4.56515315114362E-17,-0.02475000000001,
-6.77116287837691E-17));
#29131=CARTESIAN_POINT('Origin',(-4.56515315114362E-17,-0.00365,-6.77116287837691E-17));
#29132=CARTESIAN_POINT('',(-0.0137953265012258,-0.02925,-0.00170263522945406));
#29133=CARTESIAN_POINT('Origin',(-4.56515315114362E-17,-0.02475000000001,
-6.77116287837691E-17));
#29134=CARTESIAN_POINT('Origin',(-4.56515315114362E-17,-0.02925000000001,
-6.77116287837691E-17));
#29135=CARTESIAN_POINT('Origin',(-4.56515315114362E-17,-0.02925,-6.77116287837691E-17));
#29136=CARTESIAN_POINT('',(-0.007552778940802,-0.02925000000001,0.000507966801611762));
#29137=CARTESIAN_POINT('Origin',(-0.00705206865194135,-0.027,-0.000905995435036507));
#29138=CARTESIAN_POINT('Origin',(-0.0184,-0.00965,0.00149999999999993));
#29139=CARTESIAN_POINT('',(-0.0184,-0.00965,0.00149999999999993));
#29140=CARTESIAN_POINT('',(-0.0184000000000101,-0.00964999999999,0.00150000000000993));
#29141=CARTESIAN_POINT('',(-0.0184,-0.02325,0.00149999999999993));
#29142=CARTESIAN_POINT('',(-0.0184000000000101,-0.00964999999999,0.00150000000000993));
#29143=CARTESIAN_POINT('',(-0.0184000000000101,-0.02325000000001,0.00150000000000993));
#29144=CARTESIAN_POINT('Origin',(-0.0184,-0.00965,-7.10422978576446E-17));
#29145=CARTESIAN_POINT('',(-0.0184,-0.00965,-0.00150000000000007));
#29146=CARTESIAN_POINT('',(-0.0184000000000101,-0.00964999999999,-0.00150000000001007));
#29147=CARTESIAN_POINT('Origin',(-0.0184000000000101,-0.00964999999999,
-1.00710422978576E-14));
#29148=CARTESIAN_POINT('Origin',(-0.0184,-0.02325,-7.10422978576446E-17));
#29149=CARTESIAN_POINT('',(-0.0184,-0.02325,-0.00150000000000007));
#29150=CARTESIAN_POINT('Origin',(-0.0184000000000101,-0.02325000000001,
-1.00710422978576E-14));
#29151=CARTESIAN_POINT('',(-0.0184000000000101,-0.02325000000001,-0.00150000000001008));
#29152=CARTESIAN_POINT('Origin',(-0.0184,-0.02325,-0.00150000000000007));
#29153=CARTESIAN_POINT('',(-0.0184000000000101,-0.02325000000001,-0.00150000000001007));
#29154=CARTESIAN_POINT('Origin',(-4.56515315114362E-17,-0.00365,-6.77116287837691E-17));
#29155=CARTESIAN_POINT('',(-0.0116511274118543,-0.02925,0.00888108833605068));
#29156=CARTESIAN_POINT('',(-0.0132228744157255,-0.02475,0.00630698756824146));
#29157=CARTESIAN_POINT('Origin',(-4.56515315114362E-17,-0.02475000000001,
-6.77116287837691E-17));
#29158=CARTESIAN_POINT('',(-0.0088810883360508,-0.02925,0.0116511274118542));
#29159=CARTESIAN_POINT('Origin',(-4.56515315114362E-17,-0.02925000000001,
-6.77116287837691E-17));
#29160=CARTESIAN_POINT('',(-0.00630698756824158,-0.02475,0.0132228744157254));
#29161=CARTESIAN_POINT('Origin',(-4.56515315114362E-17,-0.02475000000001,
-6.77116287837691E-17));
#29162=CARTESIAN_POINT('',(-0.00630698756824158,-0.00815,0.0132228744157254));
#29163=CARTESIAN_POINT('',(-0.00630698756825158,-0.00364999999999,0.0132228744157354));
#29164=CARTESIAN_POINT('',(-0.00888108833605081,-0.00365,0.0116511274118542));
#29165=CARTESIAN_POINT('Origin',(-4.56515315114362E-17,-0.00814999999999,
-6.77116287837691E-17));
#29166=CARTESIAN_POINT('',(-0.0116511274118543,-0.00365,0.00888108833605068));
#29167=CARTESIAN_POINT('Origin',(-4.56515315114362E-17,-0.00364999999999,
-6.77116287837691E-17));
#29168=CARTESIAN_POINT('',(-0.0132228744157255,-0.00815,0.00630698756824146));
#29169=CARTESIAN_POINT('Origin',(-4.56515315114362E-17,-0.00814999999999,
-6.77116287837691E-17));
#29170=CARTESIAN_POINT('',(-0.0132228744157355,-0.00364999999999,0.00630698756825146));
#29171=CARTESIAN_POINT('',(-0.0113653314426162,-0.02325,0.00924401109905646));
#29172=CARTESIAN_POINT('',(-0.0113653314426162,-0.00965,0.00924401109905646));
#29173=CARTESIAN_POINT('',(-0.0113653314426262,-0.00364999999999,0.00924401109906646));
#29174=CARTESIAN_POINT('',(-0.00924401109905658,-0.00965,0.0113653314426161));
#29175=CARTESIAN_POINT('Ctrl Pts',(-0.0113653314426162,-0.00965,0.00924401109905647));
#29176=CARTESIAN_POINT('Ctrl Pts',(-0.0113653314426162,-0.00946151448459537,
0.00924401109905647));
#29177=CARTESIAN_POINT('Ctrl Pts',(-0.0113415286147626,-0.00926055630226629,
0.00927351838063701));
#29178=CARTESIAN_POINT('Ctrl Pts',(-0.0112435430943066,-0.00889102670991339,
0.0093920792764486));
#29179=CARTESIAN_POINT('Ctrl Pts',(-0.0111692153844281,-0.00872244398548004,
0.00948097768002287));
#29180=CARTESIAN_POINT('Ctrl Pts',(-0.0109946422781871,-0.00845623616911263,
0.00968287927809839));
#29181=CARTESIAN_POINT('Ctrl Pts',(-0.0108827047851677,-0.00834081748849188,
0.00980935406895057));
#29182=CARTESIAN_POINT('Ctrl Pts',(-0.0106316568441341,-0.00818769575944871,
0.0100809009239757));
#29183=CARTESIAN_POINT('Ctrl Pts',(-0.0104923932316729,-0.00815,0.0102258354570929));
#29184=CARTESIAN_POINT('Ctrl Pts',(-0.010225835457093,-0.00815,0.0104923932316728));
#29185=CARTESIAN_POINT('Ctrl Pts',(-0.0100809009239758,-0.00818769575944871,
0.010631656844134));
#29186=CARTESIAN_POINT('Ctrl Pts',(-0.00980935406895067,-0.00834081748849188,
0.0108827047851676));
#29187=CARTESIAN_POINT('Ctrl Pts',(-0.00968287927809849,-0.00845623616911263,
0.010994642278187));
#29188=CARTESIAN_POINT('Ctrl Pts',(-0.00948097768002297,-0.00872244398548004,
0.011169215384428));
#29189=CARTESIAN_POINT('Ctrl Pts',(-0.0093920792764487,-0.00889102670991339,
0.0112435430943065));
#29190=CARTESIAN_POINT('Ctrl Pts',(-0.0092735183806371,-0.00926055630226629,
0.0113415286147625));
#29191=CARTESIAN_POINT('Ctrl Pts',(-0.00924401109905656,-0.00946151448459537,
0.0113653314426161));
#29192=CARTESIAN_POINT('Ctrl Pts',(-0.00924401109905656,-0.00965,0.0113653314426161));
#29193=CARTESIAN_POINT('',(-0.00924401109905658,-0.02325,0.0113653314426161));
#29194=CARTESIAN_POINT('',(-0.00924401109906658,-0.00364999999999,0.0113653314426261));
#29195=CARTESIAN_POINT('Ctrl Pts',(-0.00924401109905656,-0.02325,0.0113653314426161));
#29196=CARTESIAN_POINT('Ctrl Pts',(-0.00924401109905656,-0.0234384855154046,
0.0113653314426161));
#29197=CARTESIAN_POINT('Ctrl Pts',(-0.0092735183806371,-0.0236394436977337,
0.0113415286147625));
#29198=CARTESIAN_POINT('Ctrl Pts',(-0.0093920792764487,-0.0240089732900866,
0.0112435430943065));
#29199=CARTESIAN_POINT('Ctrl Pts',(-0.00948097768002297,-0.02417755601452,
0.011169215384428));
#29200=CARTESIAN_POINT('Ctrl Pts',(-0.00968287927809848,-0.0244437638308874,
0.010994642278187));
#29201=CARTESIAN_POINT('Ctrl Pts',(-0.00980935406895067,-0.0245591825115081,
0.0108827047851676));
#29202=CARTESIAN_POINT('Ctrl Pts',(-0.0100809009239758,-0.0247123042405513,
0.010631656844134));
#29203=CARTESIAN_POINT('Ctrl Pts',(-0.010225835457093,-0.02475,0.0104923932316728));
#29204=CARTESIAN_POINT('Ctrl Pts',(-0.0104923932316729,-0.02475,0.0102258354570929));
#29205=CARTESIAN_POINT('Ctrl Pts',(-0.0106316568441341,-0.0247123042405513,
0.0100809009239757));
#29206=CARTESIAN_POINT('Ctrl Pts',(-0.0108827047851677,-0.0245591825115081,
0.00980935406895057));
#29207=CARTESIAN_POINT('Ctrl Pts',(-0.0109946422781871,-0.0244437638308874,
0.00968287927809839));
#29208=CARTESIAN_POINT('Ctrl Pts',(-0.0111692153844281,-0.02417755601452,
0.00948097768002287));
#29209=CARTESIAN_POINT('Ctrl Pts',(-0.0112435430943066,-0.0240089732900866,
0.0093920792764486));
#29210=CARTESIAN_POINT('Ctrl Pts',(-0.0113415286147626,-0.0236394436977337,
0.00927351838063701));
#29211=CARTESIAN_POINT('Ctrl Pts',(-0.0113653314426162,-0.0234384855154046,
0.00924401109905647));
#29212=CARTESIAN_POINT('Ctrl Pts',(-0.0113653314426162,-0.02325,0.00924401109905647));
#29213=CARTESIAN_POINT('Origin',(-0.0125459354524631,-0.00365,0.00598410424563523));
#29214=CARTESIAN_POINT('',(-0.0125459354524631,-0.02475,0.00598410424563523));
#29215=CARTESIAN_POINT('',(-0.00627296772624158,-0.02475000000001,0.00299205212282759));
#29216=CARTESIAN_POINT('',(-0.0125459354524631,-0.00815,0.00598410424563523));
#29217=CARTESIAN_POINT('',(-0.00627296772624158,-0.00814999999999,0.00299205212282759));
#29218=CARTESIAN_POINT('',(-0.0125459354524731,-0.00364999999999,0.00598410424564523));
#29219=CARTESIAN_POINT('Origin',(-0.00562720108101914,-0.0059,0.00434593004934238));
#29220=CARTESIAN_POINT('',(-0.0109587138343333,-0.00365,0.00855082400106514));
#29221=CARTESIAN_POINT('',(-0.0049814344358167,-0.00364999999999,0.00569980797587716));
#29222=CARTESIAN_POINT('Origin',(-4.56515315114362E-17,-0.00814999999999,
-6.77116287837691E-17));
#29223=CARTESIAN_POINT('Origin',(-4.56515315114362E-17,-0.00365,-6.77116287837691E-17));
#29224=CARTESIAN_POINT('',(-0.00855082400106526,-0.00365,0.0109587138343332));
#29225=CARTESIAN_POINT('',(-0.0058612496371804,-0.00364999999999,0.00531990391744778));
#29226=CARTESIAN_POINT('Origin',(-4.56515315114362E-17,-0.00364999999999,
-6.77116287837691E-17));
#29227=CARTESIAN_POINT('Origin',(-0.0045073717106456,-0.0059,0.00596567056265022));
#29228=CARTESIAN_POINT('',(-0.00598410424563535,-0.00815,0.012545935452463));
#29229=CARTESIAN_POINT('Origin',(-4.56515315114362E-17,-0.00814999999999,
-6.77116287837691E-17));
#29230=CARTESIAN_POINT('',(-0.00315349378413081,-0.00814999999999,0.00661143720787266));
#29231=CARTESIAN_POINT('Origin',(-0.00630698756824157,-0.00365,0.0132228744157254));
#29232=CARTESIAN_POINT('',(-0.00598410424563535,-0.02475,0.012545935452463));
#29233=CARTESIAN_POINT('',(-0.00315349378413081,-0.02475000000001,0.00661143720787266));
#29234=CARTESIAN_POINT('',(-0.00598410424564535,-0.00364999999999,0.012545935452473));
#29235=CARTESIAN_POINT('Origin',(-0.0045073717106456,-0.027,0.00596567056265022));
#29236=CARTESIAN_POINT('',(-0.00855082400106526,-0.02925,0.0109587138343332));
#29237=CARTESIAN_POINT('',(-0.00586124963718039,-0.02925000000001,0.00531990391744778));
#29238=CARTESIAN_POINT('Origin',(-4.56515315114362E-17,-0.02475000000001,
-6.77116287837691E-17));
#29239=CARTESIAN_POINT('Origin',(-4.56515315114362E-17,-0.00365,-6.77116287837691E-17));
#29240=CARTESIAN_POINT('',(-0.0109587138343333,-0.02925,0.00855082400106514));
#29241=CARTESIAN_POINT('Origin',(-4.56515315114362E-17,-0.02475000000001,
-6.77116287837691E-17));
#29242=CARTESIAN_POINT('Origin',(-4.56515315114362E-17,-0.02925000000001,
-6.77116287837691E-17));
#29243=CARTESIAN_POINT('Origin',(-4.56515315114362E-17,-0.02925,-6.77116287837691E-17));
#29244=CARTESIAN_POINT('',(-0.0049814344358167,-0.02925000000001,0.00569980797587716));
#29245=CARTESIAN_POINT('Origin',(-0.00562720108101914,-0.027,0.00434593004934238));
#29246=CARTESIAN_POINT('Origin',(-0.0119501046020527,-0.00965,0.0140714249456122));
#29247=CARTESIAN_POINT('',(-0.0119501046020527,-0.00965,0.0140714249456122));
#29248=CARTESIAN_POINT('',(-0.0119501046020627,-0.00964999999999,0.0140714249456222));
#29249=CARTESIAN_POINT('',(-0.0119501046020527,-0.02325,0.0140714249456122));
#29250=CARTESIAN_POINT('',(-0.0119501046020627,-0.00964999999999,0.0140714249456222));
#29251=CARTESIAN_POINT('',(-0.0119501046020627,-0.02325000000001,0.0140714249456222));
#29252=CARTESIAN_POINT('Origin',(-0.0130107647738325,-0.00965,0.0130107647738324));
#29253=CARTESIAN_POINT('',(-0.0140714249456123,-0.00965,0.0119501046020526));
#29254=CARTESIAN_POINT('',(-0.0140714249456223,-0.00964999999999,0.0119501046020626));
#29255=CARTESIAN_POINT('Origin',(-0.0130107647738425,-0.00964999999999,
0.0130107647738424));
#29256=CARTESIAN_POINT('Origin',(-0.0130107647738325,-0.02325,0.0130107647738324));
#29257=CARTESIAN_POINT('',(-0.0140714249456123,-0.02325,0.0119501046020526));
#29258=CARTESIAN_POINT('Origin',(-0.0130107647738425,-0.02325000000001,
0.0130107647738424));
#29259=CARTESIAN_POINT('',(-0.0140714249456223,-0.02325000000001,0.0119501046020626));
#29260=CARTESIAN_POINT('Origin',(-0.0140714249456123,-0.02325,0.0119501046020526));
#29261=CARTESIAN_POINT('',(-0.0140714249456223,-0.02325000000001,0.0119501046020626));
#29262=CARTESIAN_POINT('Origin',(-4.56515315114362E-17,-0.00365,-6.77116287837691E-17));
#29263=CARTESIAN_POINT('',(-0.00195871341465247,-0.02925,0.0145184689881288));
#29264=CARTESIAN_POINT('',(-0.00489027048777479,-0.02475,0.0138096978445003));
#29265=CARTESIAN_POINT('Origin',(-4.56515315114362E-17,-0.02475000000001,
-6.77116287837691E-17));
#29266=CARTESIAN_POINT('',(0.00195871341465238,-0.02925,0.0145184689881288));
#29267=CARTESIAN_POINT('Origin',(-4.56515315114362E-17,-0.02925000000001,
-6.77116287837691E-17));
#29268=CARTESIAN_POINT('',(0.0048902704877747,-0.02475,0.0138096978445003));
#29269=CARTESIAN_POINT('Origin',(-4.56515315114362E-17,-0.02475000000001,
-6.77116287837691E-17));
#29270=CARTESIAN_POINT('',(0.0048902704877747,-0.00815,0.0138096978445003));
#29271=CARTESIAN_POINT('',(0.00489027048778471,-0.00364999999999,0.0138096978445103));
#29272=CARTESIAN_POINT('',(0.00195871341465237,-0.00365,0.0145184689881288));
#29273=CARTESIAN_POINT('Origin',(-4.56515315114362E-17,-0.00814999999999,
-6.77116287837691E-17));
#29274=CARTESIAN_POINT('',(-0.00195871341465247,-0.00365,0.0145184689881288));
#29275=CARTESIAN_POINT('Origin',(-4.56515315114362E-17,-0.00364999999999,
-6.77116287837691E-17));
#29276=CARTESIAN_POINT('',(-0.00489027048777479,-0.00815,0.0138096978445003));
#29277=CARTESIAN_POINT('Origin',(-4.56515315114362E-17,-0.00814999999999,
-6.77116287837691E-17));
#29278=CARTESIAN_POINT('',(-0.00489027048778479,-0.00364999999999,0.0138096978445103));
#29279=CARTESIAN_POINT('',(-0.00150000000000005,-0.02325,0.0145730058670131));
#29280=CARTESIAN_POINT('',(-0.00150000000000005,-0.00965,0.0145730058670131));
#29281=CARTESIAN_POINT('',(-0.00150000000001004,-0.00364999999999,0.0145730058670231));
#29282=CARTESIAN_POINT('',(0.00149999999999995,-0.00965,0.0145730058670131));
#29283=CARTESIAN_POINT('Ctrl Pts',(-0.00150000000000005,-0.00965,0.0145730058670131));
#29284=CARTESIAN_POINT('Ctrl Pts',(-0.00150000000000005,-0.00946151448459537,
0.0145730058670131));
#29285=CARTESIAN_POINT('Ctrl Pts',(-0.00146230406011339,-0.00926055630226629,
0.0145770395249264));
#29286=CARTESIAN_POINT('Ctrl Pts',(-0.0013091826207289,-0.00889102670991339,
0.0145915885123658));
#29287=CARTESIAN_POINT('Ctrl Pts',(-0.00119376432903973,-0.00872244398548004,
0.0146018915486846));
#29288=CARTESIAN_POINT('Ctrl Pts',(-0.000927556512672315,-0.00845623616911263,
0.0146212157105804));
#29289=CARTESIAN_POINT('Ctrl Pts',(-0.000758973570028519,-0.00834081748849188,
0.0146314951324581));
#29290=CARTESIAN_POINT('Ctrl Pts',(-0.000389443245922637,-0.00818769575944871,
0.0146459900535485));
#29291=CARTESIAN_POINT('Ctrl Pts',(-0.000188484809983485,-0.00815,0.0146499999999999));
#29292=CARTESIAN_POINT('Ctrl Pts',(0.000188484809983389,-0.00815,0.0146499999999999));
#29293=CARTESIAN_POINT('Ctrl Pts',(0.000389443245922541,-0.00818769575944871,
0.0146459900535485));
#29294=CARTESIAN_POINT('Ctrl Pts',(0.000758973570028423,-0.00834081748849188,
0.0146314951324581));
#29295=CARTESIAN_POINT('Ctrl Pts',(0.000927556512672219,-0.00845623616911263,
0.0146212157105804));
#29296=CARTESIAN_POINT('Ctrl Pts',(0.00119376432903963,-0.00872244398548004,
0.0146018915486846));
#29297=CARTESIAN_POINT('Ctrl Pts',(0.00130918262072881,-0.00889102670991339,
0.0145915885123658));
#29298=CARTESIAN_POINT('Ctrl Pts',(0.00146230406011329,-0.00926055630226629,
0.0145770395249264));
#29299=CARTESIAN_POINT('Ctrl Pts',(0.00149999999999995,-0.00946151448459537,
0.0145730058670131));
#29300=CARTESIAN_POINT('Ctrl Pts',(0.00149999999999995,-0.00965,0.0145730058670131));
#29301=CARTESIAN_POINT('',(0.00149999999999995,-0.02325,0.0145730058670131));
#29302=CARTESIAN_POINT('',(0.00150000000000994,-0.00364999999999,0.0145730058670231));
#29303=CARTESIAN_POINT('Ctrl Pts',(0.00149999999999995,-0.02325,0.0145730058670131));
#29304=CARTESIAN_POINT('Ctrl Pts',(0.00149999999999995,-0.0234384855154046,
0.0145730058670131));
#29305=CARTESIAN_POINT('Ctrl Pts',(0.00146230406011329,-0.0236394436977337,
0.0145770395249264));
#29306=CARTESIAN_POINT('Ctrl Pts',(0.00130918262072881,-0.0240089732900866,
0.0145915885123658));
#29307=CARTESIAN_POINT('Ctrl Pts',(0.00119376432903963,-0.02417755601452,
0.0146018915486846));
#29308=CARTESIAN_POINT('Ctrl Pts',(0.000927556512672219,-0.0244437638308874,
0.0146212157105804));
#29309=CARTESIAN_POINT('Ctrl Pts',(0.000758973570028422,-0.0245591825115081,
0.0146314951324581));
#29310=CARTESIAN_POINT('Ctrl Pts',(0.00038944324592254,-0.0247123042405513,
0.0146459900535485));
#29311=CARTESIAN_POINT('Ctrl Pts',(0.000188484809983388,-0.02475,0.0146499999999999));
#29312=CARTESIAN_POINT('Ctrl Pts',(-0.000188484809983486,-0.02475,0.0146499999999999));
#29313=CARTESIAN_POINT('Ctrl Pts',(-0.000389443245922638,-0.0247123042405513,
0.0146459900535485));
#29314=CARTESIAN_POINT('Ctrl Pts',(-0.000758973570028519,-0.0245591825115081,
0.0146314951324581));
#29315=CARTESIAN_POINT('Ctrl Pts',(-0.000927556512672316,-0.0244437638308874,
0.0146212157105804));
#29316=CARTESIAN_POINT('Ctrl Pts',(-0.00119376432903973,-0.02417755601452,
0.0146018915486846));
#29317=CARTESIAN_POINT('Ctrl Pts',(-0.0013091826207289,-0.0240089732900866,
0.0145915885123658));
#29318=CARTESIAN_POINT('Ctrl Pts',(-0.00146230406011339,-0.0236394436977337,
0.0145770395249264));
#29319=CARTESIAN_POINT('Ctrl Pts',(-0.00150000000000005,-0.0234384855154046,
0.0145730058670131));
#29320=CARTESIAN_POINT('Ctrl Pts',(-0.00150000000000005,-0.02325,0.0145730058670131));
#29321=CARTESIAN_POINT('Origin',(-0.00463991534334946,-0.00365,0.0131027167261812));
#29322=CARTESIAN_POINT('',(-0.00463991534334946,-0.02475,0.0131027167261812));
#29323=CARTESIAN_POINT('',(-0.00231995767168476,-0.02475000000001,0.00655135836310057));
#29324=CARTESIAN_POINT('',(-0.00463991534334946,-0.00815,0.0131027167261812));
#29325=CARTESIAN_POINT('',(-0.00231995767168476,-0.00814999999999,0.00655135836310057));
#29326=CARTESIAN_POINT('',(-0.00463991534335946,-0.00364999999999,0.0131027167261912));
#29327=CARTESIAN_POINT('Origin',(-0.000905995435036485,-0.0059,0.00705206865194123));
#29328=CARTESIAN_POINT('',(-0.00170263522945404,-0.00365,0.0137953265012257));
#29329=CARTESIAN_POINT('',(0.000507966801611784,-0.00364999999999,0.00755277894080188));
#29330=CARTESIAN_POINT('Origin',(-4.56515315114362E-17,-0.00814999999999,
-6.77116287837691E-17));
#29331=CARTESIAN_POINT('Origin',(-4.56515315114362E-17,-0.00365,-6.77116287837691E-17));
#29332=CARTESIAN_POINT('',(0.00170263522945395,-0.00365,0.0137953265012257));
#29333=CARTESIAN_POINT('',(-0.000382789229399208,-0.00364999999999,0.00790626949996145));
#29334=CARTESIAN_POINT('Origin',(-4.56515315114362E-17,-0.00364999999999,
-6.77116287837691E-17));
#29335=CARTESIAN_POINT('Origin',(0.00103117300724906,-0.0059,0.0074055592111008));
#29336=CARTESIAN_POINT('',(0.00463991534334937,-0.00815,0.0131027167261812));
#29337=CARTESIAN_POINT('Origin',(-4.56515315114362E-17,-0.00814999999999,
-6.77116287837691E-17));
#29338=CARTESIAN_POINT('',(0.00244513524389734,-0.00814999999999,0.00690484892226014));
#29339=CARTESIAN_POINT('Origin',(0.0048902704877747,-0.00365,0.0138096978445003));
#29340=CARTESIAN_POINT('',(0.00463991534334937,-0.02475,0.0131027167261812));
#29341=CARTESIAN_POINT('',(0.00244513524389733,-0.02475000000001,0.00690484892226014));
#29342=CARTESIAN_POINT('',(0.00463991534335937,-0.00364999999999,0.0131027167261912));
#29343=CARTESIAN_POINT('Origin',(0.00103117300724906,-0.027,0.0074055592111008));
#29344=CARTESIAN_POINT('',(0.00170263522945395,-0.02925,0.0137953265012257));
#29345=CARTESIAN_POINT('',(-0.000382789229399207,-0.02925000000001,0.00790626949996145));
#29346=CARTESIAN_POINT('Origin',(-4.56515315114362E-17,-0.02475000000001,
-6.77116287837691E-17));
#29347=CARTESIAN_POINT('Origin',(-4.56515315114362E-17,-0.00365,-6.77116287837691E-17));
#29348=CARTESIAN_POINT('',(-0.00170263522945404,-0.02925,0.0137953265012257));
#29349=CARTESIAN_POINT('Origin',(-4.56515315114362E-17,-0.02475000000001,
-6.77116287837691E-17));
#29350=CARTESIAN_POINT('Origin',(-4.56515315114362E-17,-0.02925000000001,
-6.77116287837691E-17));
#29351=CARTESIAN_POINT('Origin',(-4.56515315114362E-17,-0.02925,-6.77116287837691E-17));
#29352=CARTESIAN_POINT('',(0.000507966801611784,-0.02925000000001,0.00755277894080188));
#29353=CARTESIAN_POINT('Origin',(-0.000905995435036485,-0.027,0.00705206865194123));
#29354=CARTESIAN_POINT('Origin',(0.00149999999999995,-0.00965,0.0184));
#29355=CARTESIAN_POINT('',(0.00149999999999995,-0.00965,0.0184));
#29356=CARTESIAN_POINT('',(0.00150000000000994,-0.00964999999999,0.01840000000001));
#29357=CARTESIAN_POINT('',(0.00149999999999995,-0.02325,0.0184));
#29358=CARTESIAN_POINT('',(0.00150000000000994,-0.00964999999999,0.01840000000001));
#29359=CARTESIAN_POINT('',(0.00150000000000994,-0.02325000000001,0.01840000000001));
#29360=CARTESIAN_POINT('Origin',(-4.89822005853117E-17,-0.00965,0.0184));
#29361=CARTESIAN_POINT('',(-0.00150000000000005,-0.00965,0.0184));
#29362=CARTESIAN_POINT('',(-0.00150000000001004,-0.00964999999999,0.01840000000001));
#29363=CARTESIAN_POINT('Origin',(-1.00489822005853E-14,-0.00964999999999,
0.01840000000001));
#29364=CARTESIAN_POINT('Origin',(-4.89822005853117E-17,-0.02325,0.0184));
#29365=CARTESIAN_POINT('',(-0.00150000000000005,-0.02325,0.0184));
#29366=CARTESIAN_POINT('Origin',(-1.00489822005853E-14,-0.02325000000001,
0.01840000000001));
#29367=CARTESIAN_POINT('',(-0.00150000000001006,-0.02325000000001,0.01840000000001));
#29368=CARTESIAN_POINT('Origin',(-0.00150000000000005,-0.02325,0.0184));
#29369=CARTESIAN_POINT('',(-0.00150000000001004,-0.02325000000001,0.01840000000001));
#29370=CARTESIAN_POINT('Origin',(-4.56515315114362E-17,-0.00365,-6.77116287837691E-17));
#29371=CARTESIAN_POINT('',(0.00888108833605071,-0.02925,0.0116511274118542));
#29372=CARTESIAN_POINT('',(0.00630698756824148,-0.02475,0.0132228744157254));
#29373=CARTESIAN_POINT('Origin',(-4.56515315114362E-17,-0.02475000000001,
-6.77116287837691E-17));
#29374=CARTESIAN_POINT('',(0.0116511274118543,-0.02925,0.00888108833605068));
#29375=CARTESIAN_POINT('Origin',(-4.56515315114362E-17,-0.02925000000001,
-6.77116287837691E-17));
#29376=CARTESIAN_POINT('',(0.0132228744157255,-0.02475,0.00630698756824146));
#29377=CARTESIAN_POINT('Origin',(-4.56515315114362E-17,-0.02475000000001,
-6.77116287837691E-17));
#29378=CARTESIAN_POINT('',(0.0132228744157255,-0.00815,0.00630698756824146));
#29379=CARTESIAN_POINT('',(0.0132228744157355,-0.00364999999999,0.00630698756825146));
#29380=CARTESIAN_POINT('',(0.0116511274118543,-0.00365,0.00888108833605069));
#29381=CARTESIAN_POINT('Origin',(-4.56515315114362E-17,-0.00814999999999,
-6.77116287837691E-17));
#29382=CARTESIAN_POINT('',(0.00888108833605071,-0.00365,0.0116511274118542));
#29383=CARTESIAN_POINT('Origin',(-4.56515315114362E-17,-0.00364999999999,
-6.77116287837691E-17));
#29384=CARTESIAN_POINT('',(0.00630698756824148,-0.00815,0.0132228744157254));
#29385=CARTESIAN_POINT('Origin',(-4.56515315114362E-17,-0.00814999999999,
-6.77116287837691E-17));
#29386=CARTESIAN_POINT('',(0.00630698756825148,-0.00364999999999,0.0132228744157354));
#29387=CARTESIAN_POINT('',(0.00924401109905649,-0.02325,0.0113653314426161));
#29388=CARTESIAN_POINT('',(0.00924401109905649,-0.00965,0.0113653314426161));
#29389=CARTESIAN_POINT('',(0.00924401109906649,-0.00364999999999,0.0113653314426261));
#29390=CARTESIAN_POINT('',(0.0113653314426162,-0.00965,0.00924401109905646));
#29391=CARTESIAN_POINT('Ctrl Pts',(0.00924401109905653,-0.00965,0.0113653314426161));
#29392=CARTESIAN_POINT('Ctrl Pts',(0.00924401109905653,-0.00946151448459537,
0.0113653314426161));
#29393=CARTESIAN_POINT('Ctrl Pts',(0.00927351838063707,-0.00926055630226629,
0.0113415286147625));
#29394=CARTESIAN_POINT('Ctrl Pts',(0.00939207927644866,-0.00889102670991339,
0.0112435430943065));
#29395=CARTESIAN_POINT('Ctrl Pts',(0.00948097768002293,-0.00872244398548004,
0.011169215384428));
#29396=CARTESIAN_POINT('Ctrl Pts',(0.00968287927809845,-0.00845623616911263,
0.010994642278187));
#29397=CARTESIAN_POINT('Ctrl Pts',(0.00980935406895063,-0.00834081748849188,
0.0108827047851675));
#29398=CARTESIAN_POINT('Ctrl Pts',(0.0100809009239757,-0.00818769575944872,
0.0106316568441339));
#29399=CARTESIAN_POINT('Ctrl Pts',(0.010225835457093,-0.00815,0.0104923932316728));
#29400=CARTESIAN_POINT('Ctrl Pts',(0.0104923932316729,-0.00815,0.0102258354570929));
#29401=CARTESIAN_POINT('Ctrl Pts',(0.0106316568441341,-0.00818769575944871,
0.0100809009239756));
#29402=CARTESIAN_POINT('Ctrl Pts',(0.0108827047851676,-0.00834081748849188,
0.00980935406895052));
#29403=CARTESIAN_POINT('Ctrl Pts',(0.0109946422781871,-0.00845623616911263,
0.00968287927809834));
#29404=CARTESIAN_POINT('Ctrl Pts',(0.0111692153844281,-0.00872244398548004,
0.00948097768002282));
#29405=CARTESIAN_POINT('Ctrl Pts',(0.0112435430943066,-0.00889102670991339,
0.00939207927644855));
#29406=CARTESIAN_POINT('Ctrl Pts',(0.0113415286147626,-0.00926055630226629,
0.00927351838063695));
#29407=CARTESIAN_POINT('Ctrl Pts',(0.0113653314426162,-0.00946151448459537,
0.00924401109905641));
#29408=CARTESIAN_POINT('Ctrl Pts',(0.0113653314426162,-0.00965,0.00924401109905641));
#29409=CARTESIAN_POINT('',(0.0113653314426162,-0.02325,0.00924401109905646));
#29410=CARTESIAN_POINT('',(0.0113653314426262,-0.00364999999999,0.00924401109906647));
#29411=CARTESIAN_POINT('Ctrl Pts',(0.0113653314426162,-0.02325,0.00924401109905641));
#29412=CARTESIAN_POINT('Ctrl Pts',(0.0113653314426162,-0.0234384855154046,
0.00924401109905641));
#29413=CARTESIAN_POINT('Ctrl Pts',(0.0113415286147626,-0.0236394436977337,
0.00927351838063695));
#29414=CARTESIAN_POINT('Ctrl Pts',(0.0112435430943066,-0.0240089732900866,
0.00939207927644855));
#29415=CARTESIAN_POINT('Ctrl Pts',(0.0111692153844281,-0.02417755601452,
0.00948097768002282));
#29416=CARTESIAN_POINT('Ctrl Pts',(0.0109946422781871,-0.0244437638308874,
0.00968287927809834));
#29417=CARTESIAN_POINT('Ctrl Pts',(0.0108827047851676,-0.0245591825115081,
0.00980935406895052));
#29418=CARTESIAN_POINT('Ctrl Pts',(0.0106316568441341,-0.0247123042405513,
0.0100809009239756));
#29419=CARTESIAN_POINT('Ctrl Pts',(0.0104923932316729,-0.02475,0.0102258354570929));
#29420=CARTESIAN_POINT('Ctrl Pts',(0.010225835457093,-0.02475,0.0104923932316728));
#29421=CARTESIAN_POINT('Ctrl Pts',(0.0100809009239757,-0.0247123042405513,
0.0106316568441339));
#29422=CARTESIAN_POINT('Ctrl Pts',(0.00980935406895063,-0.0245591825115081,
0.0108827047851675));
#29423=CARTESIAN_POINT('Ctrl Pts',(0.00968287927809845,-0.0244437638308874,
0.010994642278187));
#29424=CARTESIAN_POINT('Ctrl Pts',(0.00948097768002293,-0.02417755601452,
0.011169215384428));
#29425=CARTESIAN_POINT('Ctrl Pts',(0.00939207927644866,-0.0240089732900866,
0.0112435430943065));
#29426=CARTESIAN_POINT('Ctrl Pts',(0.00927351838063707,-0.0236394436977337,
0.0113415286147625));
#29427=CARTESIAN_POINT('Ctrl Pts',(0.00924401109905653,-0.0234384855154046,
0.0113653314426161));
#29428=CARTESIAN_POINT('Ctrl Pts',(0.00924401109905653,-0.02325,0.0113653314426161));
#29429=CARTESIAN_POINT('Origin',(0.00598410424563526,-0.00365,0.012545935452463));
#29430=CARTESIAN_POINT('',(0.00598410424563526,-0.02475,0.012545935452463));
#29431=CARTESIAN_POINT('',(0.00299205212282761,-0.02475000000001,0.00627296772624146));
#29432=CARTESIAN_POINT('',(0.00598410424563526,-0.00815,0.012545935452463));
#29433=CARTESIAN_POINT('',(0.00299205212282761,-0.00814999999999,0.00627296772624146));
#29434=CARTESIAN_POINT('',(0.00598410424564526,-0.00364999999999,0.012545935452473));
#29435=CARTESIAN_POINT('Origin',(0.0043459300493424,-0.0059,0.00562720108101902));
#29436=CARTESIAN_POINT('',(0.00855082400106517,-0.00365,0.0109587138343332));
#29437=CARTESIAN_POINT('',(0.00569980797587718,-0.00364999999999,0.00498143443581658));
#29438=CARTESIAN_POINT('Origin',(-4.56515315114362E-17,-0.00814999999999,
-6.77116287837691E-17));
#29439=CARTESIAN_POINT('Origin',(-4.56515315114362E-17,-0.00365,-6.77116287837691E-17));
#29440=CARTESIAN_POINT('',(0.0109587138343332,-0.00365,0.00855082400106514));
#29441=CARTESIAN_POINT('',(0.0053199039174478,-0.00364999999999,0.00586124963718028));
#29442=CARTESIAN_POINT('Origin',(-4.56515315114362E-17,-0.00364999999999,
-6.77116287837691E-17));
#29443=CARTESIAN_POINT('Origin',(0.00596567056265024,-0.0059,0.00450737171064548));
#29444=CARTESIAN_POINT('',(0.0125459354524631,-0.00815,0.00598410424563523));
#29445=CARTESIAN_POINT('Origin',(-4.56515315114362E-17,-0.00814999999999,
-6.77116287837691E-17));
#29446=CARTESIAN_POINT('',(0.00661143720787268,-0.00814999999999,0.0031534937841307));
#29447=CARTESIAN_POINT('Origin',(0.0132228744157255,-0.00365,0.00630698756824145));
#29448=CARTESIAN_POINT('',(0.0125459354524631,-0.02475,0.00598410424563523));
#29449=CARTESIAN_POINT('',(0.00661143720787268,-0.02475000000001,0.0031534937841307));
#29450=CARTESIAN_POINT('',(0.0125459354524731,-0.00364999999999,0.00598410424564523));
#29451=CARTESIAN_POINT('Origin',(0.00596567056265024,-0.027,0.00450737171064548));
#29452=CARTESIAN_POINT('',(0.0109587138343332,-0.02925,0.00855082400106514));
#29453=CARTESIAN_POINT('',(0.0053199039174478,-0.02925000000001,0.00586124963718027));
#29454=CARTESIAN_POINT('Origin',(-4.56515315114362E-17,-0.02475000000001,
-6.77116287837691E-17));
#29455=CARTESIAN_POINT('Origin',(-4.56515315114362E-17,-0.00365,-6.77116287837691E-17));
#29456=CARTESIAN_POINT('',(0.00855082400106517,-0.02925,0.0109587138343332));
#29457=CARTESIAN_POINT('Origin',(-4.56515315114362E-17,-0.02475000000001,
-6.77116287837691E-17));
#29458=CARTESIAN_POINT('Origin',(-4.56515315114362E-17,-0.02925000000001,
-6.77116287837691E-17));
#29459=CARTESIAN_POINT('Origin',(-4.56515315114362E-17,-0.02925,-6.77116287837691E-17));
#29460=CARTESIAN_POINT('',(0.00569980797587718,-0.02925000000001,0.00498143443581658));
#29461=CARTESIAN_POINT('Origin',(0.0043459300493424,-0.027,0.00562720108101902));
#29462=CARTESIAN_POINT('Origin',(0.0140714249456123,-0.00965,0.0119501046020526));
#29463=CARTESIAN_POINT('',(0.0140714249456123,-0.00965,0.0119501046020526));
#29464=CARTESIAN_POINT('',(0.0140714249456223,-0.00964999999999,0.0119501046020626));
#29465=CARTESIAN_POINT('',(0.0140714249456123,-0.02325,0.0119501046020526));
#29466=CARTESIAN_POINT('',(0.0140714249456223,-0.00964999999999,0.0119501046020626));
#29467=CARTESIAN_POINT('',(0.0140714249456223,-0.02325000000001,0.0119501046020626));
#29468=CARTESIAN_POINT('Origin',(0.0130107647738325,-0.00965,0.0130107647738324));
#29469=CARTESIAN_POINT('',(0.0119501046020527,-0.00965,0.0140714249456122));
#29470=CARTESIAN_POINT('',(0.0119501046020627,-0.00964999999999,0.0140714249456222));
#29471=CARTESIAN_POINT('Origin',(0.0130107647738425,-0.00964999999999,0.0130107647738424));
#29472=CARTESIAN_POINT('Origin',(0.0130107647738325,-0.02325,0.0130107647738324));
#29473=CARTESIAN_POINT('',(0.0119501046020527,-0.02325,0.0140714249456122));
#29474=CARTESIAN_POINT('Origin',(0.0130107647738425,-0.02325000000001,0.0130107647738424));
#29475=CARTESIAN_POINT('',(0.0119501046020627,-0.02325000000001,0.0140714249456222));
#29476=CARTESIAN_POINT('Origin',(0.0119501046020527,-0.02325,0.0140714249456122));
#29477=CARTESIAN_POINT('',(0.0119501046020627,-0.02325000000001,0.0140714249456222));
#29478=CARTESIAN_POINT('Origin',(-4.56515315114362E-17,-0.00365,-6.77116287837691E-17));
#29479=CARTESIAN_POINT('',(0.0145184689881289,-0.02925,0.00195871341465235));
#29480=CARTESIAN_POINT('',(0.0138096978445004,-0.02475,0.00489027048777468));
#29481=CARTESIAN_POINT('Origin',(-4.56515315114362E-17,-0.02475000000001,
-6.77116287837691E-17));
#29482=CARTESIAN_POINT('',(0.0145184689881289,-0.02925,-0.00195871341465249));
#29483=CARTESIAN_POINT('Origin',(-4.56515315114362E-17,-0.02925000000001,
-6.77116287837691E-17));
#29484=CARTESIAN_POINT('',(0.0138096978445004,-0.02475,-0.00489027048777481));
#29485=CARTESIAN_POINT('Origin',(-4.56515315114362E-17,-0.02475000000001,
-6.77116287837691E-17));
#29486=CARTESIAN_POINT('',(0.0138096978445004,-0.00815,-0.00489027048777481));
#29487=CARTESIAN_POINT('',(0.0138096978445104,-0.00364999999999,-0.00489027048778481));
#29488=CARTESIAN_POINT('',(0.0145184689881289,-0.00365,-0.00195871341465249));
#29489=CARTESIAN_POINT('Origin',(-4.56515315114362E-17,-0.00814999999999,
-6.77116287837691E-17));
#29490=CARTESIAN_POINT('',(0.0145184689881289,-0.00365,0.00195871341465235));
#29491=CARTESIAN_POINT('Origin',(-4.56515315114362E-17,-0.00364999999999,
-6.77116287837691E-17));
#29492=CARTESIAN_POINT('',(0.0138096978445004,-0.00815,0.00489027048777468));
#29493=CARTESIAN_POINT('Origin',(-4.56515315114362E-17,-0.00814999999999,
-6.77116287837691E-17));
#29494=CARTESIAN_POINT('',(0.0138096978445104,-0.00364999999999,0.00489027048778468));
#29495=CARTESIAN_POINT('',(0.0145730058670132,-0.02325,0.00149999999999993));
#29496=CARTESIAN_POINT('',(0.0145730058670132,-0.00965,0.00149999999999993));
#29497=CARTESIAN_POINT('',(0.0145730058670232,-0.00364999999999,0.00150000000000994));
#29498=CARTESIAN_POINT('',(0.0145730058670132,-0.00965,-0.00150000000000007));
#29499=CARTESIAN_POINT('Ctrl Pts',(0.0145730058670131,-0.00965,0.00149999999999993));
#29500=CARTESIAN_POINT('Ctrl Pts',(0.0145730058670131,-0.00946151448459537,
0.00149999999999993));
#29501=CARTESIAN_POINT('Ctrl Pts',(0.0145770395249264,-0.00926055630226629,
0.00146230406011328));
#29502=CARTESIAN_POINT('Ctrl Pts',(0.0145915885123658,-0.00889102670991339,
0.00130918262072879));
#29503=CARTESIAN_POINT('Ctrl Pts',(0.0146018915486847,-0.00872244398548004,
0.00119376432903961));
#29504=CARTESIAN_POINT('Ctrl Pts',(0.0146212157105804,-0.00845623616911263,
0.000927556512672201));
#29505=CARTESIAN_POINT('Ctrl Pts',(0.0146314951324581,-0.00834081748849188,
0.000758973570028406));
#29506=CARTESIAN_POINT('Ctrl Pts',(0.0146459900535485,-0.00818769575944871,
0.000389443245922524));
#29507=CARTESIAN_POINT('Ctrl Pts',(0.01465,-0.00815,0.000188484809983372));
#29508=CARTESIAN_POINT('Ctrl Pts',(0.01465,-0.00815,-0.000188484809983502));
#29509=CARTESIAN_POINT('Ctrl Pts',(0.0146459900535485,-0.00818769575944871,
-0.000389443245922654));
#29510=CARTESIAN_POINT('Ctrl Pts',(0.0146314951324581,-0.00834081748849188,
-0.000758973570028536));
#29511=CARTESIAN_POINT('Ctrl Pts',(0.0146212157105804,-0.00845623616911263,
-0.000927556512672332));
#29512=CARTESIAN_POINT('Ctrl Pts',(0.0146018915486847,-0.00872244398548004,
-0.00119376432903974));
#29513=CARTESIAN_POINT('Ctrl Pts',(0.0145915885123658,-0.00889102670991339,
-0.00130918262072892));
#29514=CARTESIAN_POINT('Ctrl Pts',(0.0145770395249264,-0.00926055630226629,
-0.00146230406011341));
#29515=CARTESIAN_POINT('Ctrl Pts',(0.0145730058670131,-0.00946151448459537,
-0.00150000000000006));
#29516=CARTESIAN_POINT('Ctrl Pts',(0.0145730058670131,-0.00965,-0.00150000000000006));
#29517=CARTESIAN_POINT('',(0.0145730058670132,-0.02325,-0.00150000000000007));
#29518=CARTESIAN_POINT('',(0.0145730058670232,-0.00364999999999,-0.00150000000001006));
#29519=CARTESIAN_POINT('Ctrl Pts',(0.0145730058670131,-0.02325,-0.00150000000000007));
#29520=CARTESIAN_POINT('Ctrl Pts',(0.0145730058670131,-0.0234384855154046,
-0.00150000000000007));
#29521=CARTESIAN_POINT('Ctrl Pts',(0.0145770395249264,-0.0236394436977337,
-0.00146230406011341));
#29522=CARTESIAN_POINT('Ctrl Pts',(0.0145915885123658,-0.0240089732900866,
-0.00130918262072892));
#29523=CARTESIAN_POINT('Ctrl Pts',(0.0146018915486847,-0.02417755601452,
-0.00119376432903974));
#29524=CARTESIAN_POINT('Ctrl Pts',(0.0146212157105804,-0.0244437638308874,
-0.000927556512672333));
#29525=CARTESIAN_POINT('Ctrl Pts',(0.0146314951324581,-0.0245591825115081,
-0.000758973570028536));
#29526=CARTESIAN_POINT('Ctrl Pts',(0.0146459900535485,-0.0247123042405513,
-0.000389443245922655));
#29527=CARTESIAN_POINT('Ctrl Pts',(0.01465,-0.02475,-0.000188484809983502));
#29528=CARTESIAN_POINT('Ctrl Pts',(0.0146499999999999,-0.02475,0.000188484809983372));
#29529=CARTESIAN_POINT('Ctrl Pts',(0.0146459900535485,-0.0247123042405513,
0.000389443245922527));
#29530=CARTESIAN_POINT('Ctrl Pts',(0.0146314951324581,-0.0245591825115081,
0.000758973570028408));
#29531=CARTESIAN_POINT('Ctrl Pts',(0.0146212157105804,-0.0244437638308874,
0.000927556512672202));
#29532=CARTESIAN_POINT('Ctrl Pts',(0.0146018915486847,-0.02417755601452,
0.00119376432903961));
#29533=CARTESIAN_POINT('Ctrl Pts',(0.0145915885123658,-0.0240089732900866,
0.00130918262072879));
#29534=CARTESIAN_POINT('Ctrl Pts',(0.0145770395249264,-0.0236394436977337,
0.00146230406011327));
#29535=CARTESIAN_POINT('Ctrl Pts',(0.0145730058670131,-0.0234384855154046,
0.00149999999999993));
#29536=CARTESIAN_POINT('Ctrl Pts',(0.0145730058670131,-0.02325,0.00149999999999993));
#29537=CARTESIAN_POINT('Origin',(0.0131027167261813,-0.00365,0.00463991534334935));
#29538=CARTESIAN_POINT('',(0.0131027167261813,-0.02475,0.00463991534334935));
#29539=CARTESIAN_POINT('',(0.00655135836310059,-0.02475000000001,0.00231995767168465));
#29540=CARTESIAN_POINT('',(0.0131027167261813,-0.00815,0.00463991534334935));
#29541=CARTESIAN_POINT('',(0.00655135836310059,-0.00814999999999,0.00231995767168465));
#29542=CARTESIAN_POINT('',(0.0131027167261912,-0.00364999999999,0.00463991534335935));
#29543=CARTESIAN_POINT('Origin',(0.00705206865194125,-0.0059,0.000905995435036372));
#29544=CARTESIAN_POINT('',(0.0137953265012258,-0.00365,0.00170263522945392));
#29545=CARTESIAN_POINT('',(0.0075527789408019,-0.00364999999999,-0.000507966801611896));
#29546=CARTESIAN_POINT('Origin',(-4.56515315114362E-17,-0.00814999999999,
-6.77116287837691E-17));
#29547=CARTESIAN_POINT('Origin',(-4.56515315114362E-17,-0.00365,-6.77116287837691E-17));
#29548=CARTESIAN_POINT('',(0.0137953265012258,-0.00365,-0.00170263522945406));
#29549=CARTESIAN_POINT('',(0.00790626949996147,-0.00364999999999,0.000382789229399096));
#29550=CARTESIAN_POINT('Origin',(-4.56515315114362E-17,-0.00364999999999,
-6.77116287837691E-17));
#29551=CARTESIAN_POINT('Origin',(0.00740555921110082,-0.0059,-0.00103117300724917));
#29552=CARTESIAN_POINT('',(0.0131027167261813,-0.00815,-0.00463991534334949));
#29553=CARTESIAN_POINT('Origin',(-4.56515315114362E-17,-0.00814999999999,
-6.77116287837691E-17));
#29554=CARTESIAN_POINT('',(0.00690484892226016,-0.00814999999999,-0.00244513524389744));
#29555=CARTESIAN_POINT('Origin',(0.0138096978445004,-0.00365,-0.00489027048777482));
#29556=CARTESIAN_POINT('',(0.0131027167261813,-0.02475,-0.00463991534334949));
#29557=CARTESIAN_POINT('',(0.00690484892226016,-0.02475000000001,-0.00244513524389744));
#29558=CARTESIAN_POINT('',(0.0131027167261912,-0.00364999999999,-0.00463991534335949));
#29559=CARTESIAN_POINT('Origin',(0.00740555921110082,-0.027,-0.00103117300724918));
#29560=CARTESIAN_POINT('',(0.0137953265012258,-0.02925,-0.00170263522945406));
#29561=CARTESIAN_POINT('',(0.00790626949996147,-0.02925000000001,0.000382789229399094));
#29562=CARTESIAN_POINT('Origin',(-4.56515315114362E-17,-0.02475000000001,
-6.77116287837691E-17));
#29563=CARTESIAN_POINT('Origin',(-4.56515315114362E-17,-0.00365,-6.77116287837691E-17));
#29564=CARTESIAN_POINT('',(0.0137953265012258,-0.02925,0.00170263522945392));
#29565=CARTESIAN_POINT('Origin',(-4.56515315114362E-17,-0.02475000000001,
-6.77116287837691E-17));
#29566=CARTESIAN_POINT('Origin',(-4.56515315114362E-17,-0.02925000000001,
-6.77116287837691E-17));
#29567=CARTESIAN_POINT('Origin',(-4.56515315114362E-17,-0.02925,-6.77116287837691E-17));
#29568=CARTESIAN_POINT('',(0.0075527789408019,-0.02925000000001,-0.000507966801611896));
#29569=CARTESIAN_POINT('Origin',(0.00705206865194125,-0.027,0.000905995435036372));
#29570=CARTESIAN_POINT('Origin',(0.0184,-0.00965,-0.00150000000000007));
#29571=CARTESIAN_POINT('',(0.0184,-0.00965,-0.00150000000000007));
#29572=CARTESIAN_POINT('',(0.01840000000001,-0.00964999999999,-0.00150000000001006));
#29573=CARTESIAN_POINT('',(0.0184,-0.02325,-0.00150000000000007));
#29574=CARTESIAN_POINT('',(0.01840000000001,-0.00964999999999,-0.00150000000001006));
#29575=CARTESIAN_POINT('',(0.01840000000001,-0.02325000000001,-0.00150000000001006));
#29576=CARTESIAN_POINT('Origin',(0.0184,-0.00965,-6.43809597098936E-17));
#29577=CARTESIAN_POINT('',(0.0184,-0.00965,0.00149999999999993));
#29578=CARTESIAN_POINT('',(0.01840000000001,-0.00964999999999,0.00150000000000994));
#29579=CARTESIAN_POINT('Origin',(0.01840000000001,-0.00964999999999,9.93561904029011E-15));
#29580=CARTESIAN_POINT('Origin',(0.0184,-0.02325,-6.43809597098936E-17));
#29581=CARTESIAN_POINT('',(0.0184,-0.024,-0.00129903810567673));
#29582=CARTESIAN_POINT('Origin',(0.01840000000001,-0.02325000000001,9.93561904029011E-15));
#29583=CARTESIAN_POINT('',(0.0184,-0.024,0.00129903810567659));
#29584=CARTESIAN_POINT('Origin',(0.01840000000001,-0.02325000000001,9.93561904029011E-15));
#29585=CARTESIAN_POINT('',(0.0184,-0.02325,0.00149999999999993));
#29586=CARTESIAN_POINT('Origin',(0.01840000000001,-0.02325000000001,9.93561904029011E-15));
#29587=CARTESIAN_POINT('',(0.01840000000001,-0.02325000000001,0.00150000000000994));
#29588=CARTESIAN_POINT('Origin',(0.0184,-0.02325,0.00149999999999993));
#29589=CARTESIAN_POINT('',(0.01840000000001,-0.02325000000001,0.00150000000000994));
#29590=CARTESIAN_POINT('Origin',(-4.78719775606865E-17,-0.00365,-6.88218518083943E-17));
#29591=CARTESIAN_POINT('',(0.01915,-0.00365,0.00793218971944471));
#29592=CARTESIAN_POINT('',(0.01915,-0.00365,-0.00793218971944484));
#29593=CARTESIAN_POINT('',(0.01915000000001,-0.00364999999999,0.00793218971945471));
#29594=CARTESIAN_POINT('',(0.00793218971944474,-0.00365,-0.01915));
#29595=CARTESIAN_POINT('',(0.01915000000001,-0.00364999999999,-0.00793218971945484));
#29596=CARTESIAN_POINT('',(-0.00793218971944482,-0.00365,-0.01915));
#29597=CARTESIAN_POINT('',(0.00793218971945473,-0.00364999999999,-0.0191500000000101));
#29598=CARTESIAN_POINT('',(-0.01915,-0.00365,-0.00793218971944485));
#29599=CARTESIAN_POINT('',(-0.00793218971945482,-0.00364999999999,-0.0191500000000101));
#29600=CARTESIAN_POINT('',(-0.01915,-0.00365,0.0079321897194447));
#29601=CARTESIAN_POINT('',(-0.0191500000000101,-0.00364999999999,-0.00793218971945485));
#29602=CARTESIAN_POINT('',(-0.00793218971944483,-0.00365,0.01915));
#29603=CARTESIAN_POINT('',(-0.0191500000000101,-0.00364999999999,0.0079321897194547));
#29604=CARTESIAN_POINT('',(0.00793218971944473,-0.00365,0.01915));
#29605=CARTESIAN_POINT('',(-0.00793218971945483,-0.00364999999999,0.01915000000001));
#29606=CARTESIAN_POINT('',(0.00793218971945473,-0.00364999999999,0.01915000000001));
#29607=CARTESIAN_POINT('',(0.0184,-0.00365,-0.00762152954766502));
#29608=CARTESIAN_POINT('',(0.0184,-0.00365,0.00762152954766488));
#29609=CARTESIAN_POINT('',(0.01840000000001,-0.00364999999999,-0.00762152954767502));
#29610=CARTESIAN_POINT('',(0.0076215295476649,-0.00365,0.0184));
#29611=CARTESIAN_POINT('',(0.01840000000001,-0.00364999999999,0.00762152954767488));
#29612=CARTESIAN_POINT('',(-0.007621529547665,-0.00365,0.0184));
#29613=CARTESIAN_POINT('',(0.0076215295476749,-0.00364999999999,0.01840000000001));
#29614=CARTESIAN_POINT('',(-0.0184,-0.00365,0.00762152954766489));
#29615=CARTESIAN_POINT('',(-0.007621529547675,-0.00364999999999,0.01840000000001));
#29616=CARTESIAN_POINT('',(-0.0184,-0.00365,-0.00762152954766502));
#29617=CARTESIAN_POINT('',(-0.0184000000000101,-0.00364999999999,0.00762152954767489));
#29618=CARTESIAN_POINT('',(-0.007621529547665,-0.00365,-0.0184));
#29619=CARTESIAN_POINT('',(-0.0184000000000101,-0.00364999999999,-0.00762152954767502));
#29620=CARTESIAN_POINT('',(0.00762152954766491,-0.00365,-0.0184));
#29621=CARTESIAN_POINT('',(-0.007621529547675,-0.00364999999999,-0.0184000000000101));
#29622=CARTESIAN_POINT('',(0.00762152954767491,-0.00364999999999,-0.0184000000000101));
#29623=CARTESIAN_POINT('Origin',(-0.01915,-0.01645,0.0079321897194447));
#29624=CARTESIAN_POINT('',(-0.00793218971944483,-0.02925,0.01915));
#29625=CARTESIAN_POINT('',(-0.00793218971945483,-0.01645,0.01915000000001));
#29626=CARTESIAN_POINT('',(-0.01915,-0.02925,0.0079321897194447));
#29627=CARTESIAN_POINT('',(-0.0191500000000101,-0.01645,0.0079321897194547));
#29628=CARTESIAN_POINT('',(-0.0191500000000101,-0.02925000000001,0.0079321897194547));
#29629=CARTESIAN_POINT('Origin',(-0.00793218971944483,-0.01645,0.01915));
#29630=CARTESIAN_POINT('',(0.00793218971944473,-0.02925,0.01915));
#29631=CARTESIAN_POINT('',(0.00793218971945473,-0.01645,0.01915000000001));
#29632=CARTESIAN_POINT('',(-0.00793218971945483,-0.02925000000001,0.01915000000001));
#29633=CARTESIAN_POINT('Origin',(0.00793218971944473,-0.01645,0.01915));
#29634=CARTESIAN_POINT('',(0.01915,-0.02925,0.00793218971944471));
#29635=CARTESIAN_POINT('',(0.01915,-0.024,0.00793218971944471));
#29636=CARTESIAN_POINT('',(0.01915000000001,-0.01645,0.00793218971945471));
#29637=CARTESIAN_POINT('',(0.01915000000001,-0.01645,0.00793218971945471));
#29638=CARTESIAN_POINT('',(0.00793218971945473,-0.02925000000001,0.01915000000001));
#29639=CARTESIAN_POINT('Origin',(0.01915,-0.01645,-0.00793218971944484));
#29640=CARTESIAN_POINT('',(0.00793218971944474,-0.02925,-0.01915));
#29641=CARTESIAN_POINT('',(0.00793218971945474,-0.01645,-0.0191500000000101));
#29642=CARTESIAN_POINT('',(0.01915,-0.024,-0.00793218971944484));
#29643=CARTESIAN_POINT('',(0.01915000000001,-0.01645,-0.00793218971945484));
#29644=CARTESIAN_POINT('',(0.01915,-0.02925,-0.00793218971944484));
#29645=CARTESIAN_POINT('',(0.01915000000001,-0.01645,-0.00793218971945484));
#29646=CARTESIAN_POINT('',(0.01915000000001,-0.02925000000001,-0.00793218971945484));
#29647=CARTESIAN_POINT('Origin',(0.00793218971944474,-0.01645,-0.01915));
#29648=CARTESIAN_POINT('',(-0.00793218971944482,-0.02925,-0.01915));
#29649=CARTESIAN_POINT('',(-0.00793218971945482,-0.01645,-0.0191500000000101));
#29650=CARTESIAN_POINT('',(0.00793218971945473,-0.02925000000001,-0.0191500000000101));
#29651=CARTESIAN_POINT('Origin',(-0.00793218971944482,-0.01645,-0.01915));
#29652=CARTESIAN_POINT('',(-0.01915,-0.02925,-0.00793218971944485));
#29653=CARTESIAN_POINT('',(-0.0191500000000101,-0.01645,-0.00793218971945485));
#29654=CARTESIAN_POINT('',(-0.00793218971945482,-0.02925000000001,-0.0191500000000101));
#29655=CARTESIAN_POINT('Origin',(-0.01915,-0.01645,-0.00793218971944485));
#29656=CARTESIAN_POINT('',(-0.0191500000000101,-0.02925000000001,-0.00793218971945485));
#29657=CARTESIAN_POINT('Origin',(-4.78719775606865E-17,-0.02925,-6.88218518083943E-17));
#29658=CARTESIAN_POINT('',(0.02715,-0.02925,-0.00793218971944484));
#29659=CARTESIAN_POINT('',(0.01915000000001,-0.02925000000001,-0.00793218971945484));
#29660=CARTESIAN_POINT('',(0.02715,-0.02925,0.00793218971943127));
#29661=CARTESIAN_POINT('',(0.02715000000001,-0.02925000000001,0.00793218971944127));
#29662=CARTESIAN_POINT('',(0.01915000000001,-0.02925000000001,0.00793218971944127));
#29663=CARTESIAN_POINT('',(0.0224,-0.02925,-0.00718218971944484));
#29664=CARTESIAN_POINT('',(0.0184,-0.02925,-0.00718218971944484));
#29665=CARTESIAN_POINT('',(0.01120000000001,-0.02925000000001,-0.00718218971945484));
#29666=CARTESIAN_POINT('',(0.0184,-0.02925,-0.00762152954766502));
#29667=CARTESIAN_POINT('',(0.01840000000001,-0.02925000000001,-0.00762152954767502));
#29668=CARTESIAN_POINT('',(0.00762152954766491,-0.02925,-0.0184));
#29669=CARTESIAN_POINT('',(0.00762152954767491,-0.02925000000001,-0.0184000000000101));
#29670=CARTESIAN_POINT('',(-0.007621529547665,-0.02925,-0.0184));
#29671=CARTESIAN_POINT('',(-0.007621529547675,-0.02925000000001,-0.0184000000000101));
#29672=CARTESIAN_POINT('',(-0.0184,-0.02925,-0.00762152954766502));
#29673=CARTESIAN_POINT('',(-0.0184000000000101,-0.02925000000001,-0.00762152954767502));
#29674=CARTESIAN_POINT('',(-0.0184,-0.02925,0.00762152954766489));
#29675=CARTESIAN_POINT('',(-0.0184000000000101,-0.02925000000001,0.00762152954767489));
#29676=CARTESIAN_POINT('',(-0.007621529547665,-0.02925,0.0184));
#29677=CARTESIAN_POINT('',(-0.007621529547675,-0.02925000000001,0.01840000000001));
#29678=CARTESIAN_POINT('',(0.0076215295476649,-0.02925,0.0184));
#29679=CARTESIAN_POINT('',(0.0076215295476749,-0.02925000000001,0.01840000000001));
#29680=CARTESIAN_POINT('',(0.0184,-0.02925,0.00762152954766488));
#29681=CARTESIAN_POINT('',(0.01840000000001,-0.02925000000001,0.00762152954767488));
#29682=CARTESIAN_POINT('',(0.0184,-0.02925,0.00718218971944471));
#29683=CARTESIAN_POINT('',(0.01840000000001,-0.02925000000001,-0.00762152954767502));
#29684=CARTESIAN_POINT('',(0.0224,-0.02925,0.00718218971944471));
#29685=CARTESIAN_POINT('',(0.00920000000000996,-0.02925000000001,0.00718218971945471));
#29686=CARTESIAN_POINT('',(0.02240000000001,-0.02925000000001,0.00359109485973232));
#29687=CARTESIAN_POINT('Origin',(0.0184,-0.01645,0.00762152954766488));
#29688=CARTESIAN_POINT('',(0.01840000000001,-0.01645,0.00762152954767488));
#29689=CARTESIAN_POINT('',(0.0076215295476749,-0.01645,0.01840000000001));
#29690=CARTESIAN_POINT('Origin',(0.0076215295476649,-0.01645,0.0184));
#29691=CARTESIAN_POINT('',(-0.007621529547675,-0.01645,0.01840000000001));
#29692=CARTESIAN_POINT('Origin',(-0.007621529547665,-0.01645,0.0184));
#29693=CARTESIAN_POINT('',(-0.0184000000000101,-0.01645,0.00762152954767489));
#29694=CARTESIAN_POINT('Origin',(-0.0184,-0.01645,0.00762152954766489));
#29695=CARTESIAN_POINT('',(-0.0184000000000101,-0.01645,-0.00762152954767502));
#29696=CARTESIAN_POINT('Origin',(-0.0184,-0.01645,-0.00762152954766502));
#29697=CARTESIAN_POINT('',(-0.007621529547675,-0.01645,-0.0184000000000101));
#29698=CARTESIAN_POINT('Origin',(-0.007621529547665,-0.01645,-0.0184));
#29699=CARTESIAN_POINT('',(0.00762152954767491,-0.01645,-0.0184000000000101));
#29700=CARTESIAN_POINT('Origin',(0.00762152954766491,-0.01645,-0.0184));
#29701=CARTESIAN_POINT('',(0.01840000000001,-0.01645,-0.00762152954767502));
#29702=CARTESIAN_POINT('Origin',(0.01915,-0.024,0.00718218971944471));
#29703=CARTESIAN_POINT('',(0.0184,-0.024,-0.00718218971944484));
#29704=CARTESIAN_POINT('',(0.01840000000001,-0.02400000000001,-0.000219669914120157));
#29705=CARTESIAN_POINT('',(0.01915,-0.024,-0.00718218971944484));
#29706=CARTESIAN_POINT('',(0.01915000000001,-0.02400000000001,-0.00718218971945484));
#29707=CARTESIAN_POINT('',(0.01915,-0.024,0.00718218971944471));
#29708=CARTESIAN_POINT('',(0.01915000000001,-0.02400000000001,0.00755718971945471));
#29709=CARTESIAN_POINT('',(0.0184,-0.024,0.00718218971944471));
#29710=CARTESIAN_POINT('',(0.01915000000001,-0.02400000000001,0.00718218971945471));
#29711=CARTESIAN_POINT('',(0.01840000000001,-0.02400000000001,-0.000219669914120157));
#29712=CARTESIAN_POINT('',(0.01840000000001,-0.02400000000001,0.00359109485973232));
#29713=CARTESIAN_POINT('Origin',(0.01915,-0.024,-0.00718218971944484));
#29714=CARTESIAN_POINT('',(0.02715,-0.0285,-0.00718218971944484));
#29715=CARTESIAN_POINT('',(0.0224,-0.0285,-0.00718218971944484));
#29716=CARTESIAN_POINT('',(0.01915000000001,-0.02850000000001,-0.00718218971945484));
#29717=CARTESIAN_POINT('',(0.02715,-0.024,-0.00718218971944484));
#29718=CARTESIAN_POINT('',(0.02715000000001,-0.02400000000001,-0.00718218971945484));
#29719=CARTESIAN_POINT('',(0.01915000000001,-0.02400000000001,-0.00718218971945484));
#29720=CARTESIAN_POINT('',(0.01840000000001,-0.02285000000001,-0.00718218971945484));
#29721=CARTESIAN_POINT('',(0.02240000000001,-0.02925000000001,-0.00718218971945484));
#29722=CARTESIAN_POINT('Origin',(0.01915,-0.0285,0.00718218971944471));
#29723=CARTESIAN_POINT('',(0.02715,-0.024,0.00718218971944471));
#29724=CARTESIAN_POINT('',(0.01915000000001,-0.02400000000001,0.00718218971945471));
#29725=CARTESIAN_POINT('',(0.02715,-0.0285,0.00718218971944471));
#29726=CARTESIAN_POINT('',(0.02715000000001,-0.02850000000001,0.00718218971945471));
#29727=CARTESIAN_POINT('',(0.0224,-0.0285,0.00718218971944471));
#29728=CARTESIAN_POINT('',(0.01915000000001,-0.02850000000001,0.00718218971945471));
#29729=CARTESIAN_POINT('',(0.02240000000001,-0.02925000000001,0.00718218971945471));
#29730=CARTESIAN_POINT('',(0.01840000000001,-0.02247500000001,0.00718218971945471));
#29731=CARTESIAN_POINT('Origin',(0.0184,-0.02625,-6.57011291170234E-17));
#29732=CARTESIAN_POINT('Origin',(0.02715,-0.026625,-6.32707366852685E-17));
#29733=CARTESIAN_POINT('',(0.02715,-0.024,-0.00793218971944484));
#29734=CARTESIAN_POINT('',(0.02715000000001,-0.02400000000001,-0.00793218971945484));
#29735=CARTESIAN_POINT('',(0.02715000000001,-0.02850000000001,-0.00718218971945484));
#29736=CARTESIAN_POINT('',(0.02715,-0.024,0.00793218971944471));
#29737=CARTESIAN_POINT('',(0.02715000000001,-0.02400000000001,0.00718218971945471));
#29738=CARTESIAN_POINT('',(0.02715000000001,-0.02400000000001,0.00793218971945471));
#29739=CARTESIAN_POINT('',(0.02715000000001,-0.02925000000001,-0.00793218971945484));
#29740=CARTESIAN_POINT('Origin',(0.01915,-0.024,-0.00793218971944484));
#29741=CARTESIAN_POINT('',(0.01915000000001,-0.02400000000001,9.93506392877779E-15));
#29742=CARTESIAN_POINT('',(0.01915000000001,-0.02400000000001,-0.00793218971945484));
#29743=CARTESIAN_POINT('Origin',(0.01915,-0.024,0.00718218971944471));
#29744=CARTESIAN_POINT('',(0.01915000000001,-0.02400000000001,0.00755718971945471));
#29745=CARTESIAN_POINT('',(0.01915000000001,-0.02400000000001,0.00793218971945471));
#29746=CARTESIAN_POINT('Origin',(0.01915,-0.024,0.00793218971944471));
#29747=CARTESIAN_POINT('Origin',(0.01915,-0.02925,-0.00793218971944484));
#29748=CARTESIAN_POINT('Origin',(0.0184,-0.01645,-0.00762152954766502));
#29749=CARTESIAN_POINT('Origin',(0.01915,-0.01645,0.00793218971944471));
#29750=CARTESIAN_POINT('Origin',(0.01915,-0.0285,-0.00718218971944484));
#29751=CARTESIAN_POINT('',(0.02240000000001,-0.02850000000001,9.93612102271845E-15));
#29752=CARTESIAN_POINT('Origin',(0.0224,-0.02925,0.00718218971944471));
#29753=CARTESIAN_POINT('',(0.,0.,0.));
#29754=CARTESIAN_POINT('Origin',(0.0121040592752336,-0.01,0.00446113764208535));
#29755=CARTESIAN_POINT('',(0.0119220873914306,-0.0225,0.0049268481031072));
#29756=CARTESIAN_POINT('',(0.0119220873914306,-0.017,0.0049268481031072));
#29757=CARTESIAN_POINT('',(0.0119220873914382,-0.01000000000001,0.00492684810311909));
#29758=CARTESIAN_POINT('',(0.0122678470666214,-0.0225,0.00398872515347788));
#29759=CARTESIAN_POINT('Origin',(0.0121040592752413,-0.02250000000001,0.00446113764209724));
#29760=CARTESIAN_POINT('',(0.0122678470666214,-0.017,0.00398872515347788));
#29761=CARTESIAN_POINT('',(0.0122678470666291,-0.01000000000001,0.00398872515348977));
#29762=CARTESIAN_POINT('Origin',(0.0121040592752413,-0.01700000000001,0.00446113764209724));
#29763=CARTESIAN_POINT('Origin',(0.0113653930429603,-0.01,0.00610228162075688));
#29764=CARTESIAN_POINT('',(0.0111203777280115,-0.0225,0.00653813422822932));
#29765=CARTESIAN_POINT('',(0.0111203777280115,-0.017,0.00653813422822932));
#29766=CARTESIAN_POINT('',(0.0111203777280192,-0.01000000000001,0.00653813422824121));
#29767=CARTESIAN_POINT('',(0.0115933339737932,-0.0225,0.00565726147284101));
#29768=CARTESIAN_POINT('Origin',(0.011365393042968,-0.02250000000001,0.00610228162076877));
#29769=CARTESIAN_POINT('',(0.0115933339737932,-0.017,0.00565726147284101));
#29770=CARTESIAN_POINT('',(0.0115933339738008,-0.01000000000001,0.0056572614728529));
#29771=CARTESIAN_POINT('Origin',(0.011365393042968,-0.01700000000001,0.00610228162076877));
#29772=CARTESIAN_POINT('Origin',(0.0104055123630489,-0.01,0.00762465162892286));
#29773=CARTESIAN_POINT('',(0.010102222561359,-0.0225,0.00802216300761644));
#29774=CARTESIAN_POINT('',(0.010102222561359,-0.017,0.00802216300761644));
#29775=CARTESIAN_POINT('',(0.0101022225613666,-0.01000000000001,0.00802216300762832));
#29776=CARTESIAN_POINT('',(0.0106931698223871,-0.0225,0.00721568563267486));
#29777=CARTESIAN_POINT('Origin',(0.0104055123630566,-0.02250000000001,0.00762465162893475));
#29778=CARTESIAN_POINT('',(0.0106931698223871,-0.017,0.00721568563267486));
#29779=CARTESIAN_POINT('',(0.0106931698223947,-0.01000000000001,0.00721568563268675));
#29780=CARTESIAN_POINT('Origin',(0.0104055123630566,-0.01700000000001,0.00762465162893475));
#29781=CARTESIAN_POINT('Origin',(0.00924310022108555,-0.01,0.00899861646604452));
#29782=CARTESIAN_POINT('',(0.00888743912365737,-0.0225,0.00935004950913547));
#29783=CARTESIAN_POINT('',(0.00888743912365737,-0.017,0.00935004950913547));
#29784=CARTESIAN_POINT('',(0.00888743912366502,-0.01000000000001,0.00935004950914736));
#29785=CARTESIAN_POINT('',(0.00958487528368847,-0.0225,0.00863366467938941));
#29786=CARTESIAN_POINT('Origin',(0.00924310022109321,-0.02250000000001,
0.00899861646605642));
#29787=CARTESIAN_POINT('',(0.00958487528368847,-0.017,0.00863366467938941));
#29788=CARTESIAN_POINT('',(0.00958487528369612,-0.01000000000001,0.00863366467940131));
#29789=CARTESIAN_POINT('Origin',(0.00924310022109321,-0.01700000000001,
0.00899861646605642));
#29790=CARTESIAN_POINT('Origin',(0.00790078164718944,-0.01,0.0101974334694291));
#29791=CARTESIAN_POINT('',(0.0074996717927259,-0.0225,0.0104959479324828));
#29792=CARTESIAN_POINT('',(0.0074996717927259,-0.017,0.0104959479324828));
#29793=CARTESIAN_POINT('',(0.00749967179273355,-0.01000000000001,0.0104959479324947));
#29794=CARTESIAN_POINT('',(0.00829002205022697,-0.0225,0.00988359926376768));
#29795=CARTESIAN_POINT('Origin',(0.0079007816471971,-0.02250000000001,0.010197433469441));
#29796=CARTESIAN_POINT('',(0.00829002205022697,-0.017,0.00988359926376768));
#29797=CARTESIAN_POINT('',(0.00829002205023463,-0.01000000000001,0.00988359926377957));
#29798=CARTESIAN_POINT('Origin',(0.0079007816471971,-0.01700000000001,0.010197433469441));
#29799=CARTESIAN_POINT('Origin',(0.00640468334553672,-0.01,0.01119776902974));
#29800=CARTESIAN_POINT('',(0.00596593188109928,-0.0225,0.0114375546682883));
#29801=CARTESIAN_POINT('',(0.00596593188109928,-0.017,0.0114375546682883));
#29802=CARTESIAN_POINT('',(0.00596593188110694,-0.01000000000001,0.0114375546683002));
#29803=CARTESIAN_POINT('',(0.00683381296731816,-0.0225,0.0109411608309043));
#29804=CARTESIAN_POINT('Origin',(0.00640468334554438,-0.02250000000001,
0.0111977690297519));
#29805=CARTESIAN_POINT('',(0.00683381296731816,-0.017,0.0109411608309043));
#29806=CARTESIAN_POINT('',(0.00683381296732582,-0.01000000000001,0.0109411608309161));
#29807=CARTESIAN_POINT('Origin',(0.00640468334554438,-0.01700000000001,
0.0111977690297519));
#29808=CARTESIAN_POINT('Origin',(0.00478392516778247,-0.01,0.0119801527531604));
#29809=CARTESIAN_POINT('',(0.004316071891554,-0.0225,0.0121565424125011));
#29810=CARTESIAN_POINT('',(0.004316071891554,-0.017,0.0121565424125011));
#29811=CARTESIAN_POINT('',(0.00431607189156165,-0.01000000000001,0.012156542412513));
#29812=CARTESIAN_POINT('',(0.00524459148834751,-0.0225,0.0117857651478533));
#29813=CARTESIAN_POINT('Origin',(0.00478392516779012,-0.02250000000001,
0.0119801527531723));
#29814=CARTESIAN_POINT('',(0.00524459148834751,-0.017,0.0117857651478533));
#29815=CARTESIAN_POINT('',(0.00524459148835515,-0.01000000000001,0.0117857651478652));
#29816=CARTESIAN_POINT('Origin',(0.00478392516779012,-0.01700000000001,
0.0119801527531723));
#29817=CARTESIAN_POINT('Origin',(0.00307005332827152,-0.01,0.0125293564304624));
#29818=CARTESIAN_POINT('',(0.00258220447209863,-0.0225,0.0126389168865166));
#29819=CARTESIAN_POINT('',(0.00258220447209863,-0.017,0.0126389168865166));
#29820=CARTESIAN_POINT('',(0.00258220447210628,-0.01000000000001,0.0126389168865285));
#29821=CARTESIAN_POINT('',(0.00355329000169056,-0.0225,0.0124009729523085));
#29822=CARTESIAN_POINT('Origin',(0.00307005332827917,-0.02250000000001,
0.0125293564304743));
#29823=CARTESIAN_POINT('',(0.00355329000169056,-0.017,0.0124009729523085));
#29824=CARTESIAN_POINT('',(0.00355329000169822,-0.01000000000001,0.0124009729523203));
#29825=CARTESIAN_POINT('Origin',(0.00307005332827917,-0.01700000000001,
0.0125293564304743));
#29826=CARTESIAN_POINT('Origin',(0.00129642639285968,-0.01,0.0128346904367771));
#29827=CARTESIAN_POINT('',(0.000798077379807919,-0.0225,0.0128752892198909));
#29828=CARTESIAN_POINT('',(0.000798077379807918,-0.017,0.0128752892198909));
#29829=CARTESIAN_POINT('',(0.000798077379815572,-0.01000000000001,0.0128752892199028));
#29830=CARTESIAN_POINT('',(0.00179282776695818,-0.0225,0.0127748099241446));
#29831=CARTESIAN_POINT('Origin',(0.00129642639286733,-0.02250000000001,
0.012834690436789));
#29832=CARTESIAN_POINT('',(0.00179282776695818,-0.017,0.0127748099241446));
#29833=CARTESIAN_POINT('',(0.00179282776696584,-0.01000000000001,0.0127748099241565));
#29834=CARTESIAN_POINT('Origin',(0.00129642639286733,-0.01700000000001,
0.012834690436789));
#29835=CARTESIAN_POINT('Origin',(-0.000502434007626007,-0.01,0.0128902117929839));
#29836=CARTESIAN_POINT('',(-0.00100158338088122,-0.0225,0.0128610586940245));
#29837=CARTESIAN_POINT('',(-0.00100158338088122,-0.017,0.0128610586940245));
#29838=CARTESIAN_POINT('',(-0.00100158338087356,-0.01000000000001,0.0128610586940364));
#29839=CARTESIAN_POINT('',(-2.52982094668671E-6,-0.0225,0.0128999997519382));
#29840=CARTESIAN_POINT('Origin',(-0.000502434007618352,-0.02250000000001,
0.0128902117929958));
#29841=CARTESIAN_POINT('',(-2.52982094668715E-6,-0.017,0.0128999997519382));
#29842=CARTESIAN_POINT('',(-2.52982093903355E-6,-0.01000000000001,0.0128999997519501));
#29843=CARTESIAN_POINT('Origin',(-0.000502434007618352,-0.01700000000001,
0.0128902117929958));
#29844=CARTESIAN_POINT('Origin',(-0.00229151510166345,-0.01,0.0126948398390388));
#29845=CARTESIAN_POINT('',(-0.00278174946034568,-0.0225,0.0125965022899163));
#29846=CARTESIAN_POINT('',(-0.00278174946034568,-0.017,0.0125965022899163));
#29847=CARTESIAN_POINT('',(-0.00278174946035758,-0.01000000000001,0.012596502289924));
#29848=CARTESIAN_POINT('',(-0.00179783816876445,-0.0225,0.0127741057580926));
#29849=CARTESIAN_POINT('Origin',(-0.00229151510165579,-0.02250000000001,
0.0126948398390507));
#29850=CARTESIAN_POINT('',(-0.00179783816876445,-0.017,0.0127741057580926));
#29851=CARTESIAN_POINT('',(-0.0017978381687568,-0.01000000000001,0.0127741057581045));
#29852=CARTESIAN_POINT('Origin',(-0.00229151510165579,-0.01700000000001,
0.0126948398390507));
#29853=CARTESIAN_POINT('Origin',(-0.00403599446080683,-0.01,0.0122523772677932));
#29854=CARTESIAN_POINT('',(-0.00450777195075764,-0.0225,0.0120867692970439));
#29855=CARTESIAN_POINT('',(-0.00450777195075764,-0.017,0.0120867692970439));
#29856=CARTESIAN_POINT('',(-0.00450777195076953,-0.01000000000001,0.0120867692970515));
#29857=CARTESIAN_POINT('',(-0.00355815364163782,-0.0225,0.0123995783259956));
#29858=CARTESIAN_POINT('Origin',(-0.00403599446081873,-0.02250000000001,
0.0122523772678009));
#29859=CARTESIAN_POINT('',(-0.00355815364163782,-0.017,0.0123995783259956));
#29860=CARTESIAN_POINT('',(-0.00355815364164971,-0.01000000000001,0.0123995783260032));
#29861=CARTESIAN_POINT('Origin',(-0.00403599446081873,-0.01700000000001,
0.0122523772678009));
#29862=CARTESIAN_POINT('Origin',(-0.00570191777864627,-0.01,0.0115714361099027));
#29863=CARTESIAN_POINT('',(-0.00614605578766269,-0.0225,0.0113417810883008));
#29864=CARTESIAN_POINT('',(-0.0061460557876627,-0.017,0.0113417810883008));
#29865=CARTESIAN_POINT('',(-0.00614605578767459,-0.01000000000001,0.0113417810883085));
#29866=CARTESIAN_POINT('',(-0.0052492137012165,-0.0225,0.0117837072060944));
#29867=CARTESIAN_POINT('Origin',(-0.00570191777865816,-0.02250000000001,
0.0115714361099103));
#29868=CARTESIAN_POINT('',(-0.0052492137012165,-0.017,0.0117837072060944));
#29869=CARTESIAN_POINT('',(-0.00524921370122839,-0.01000000000001,0.0117837072061021));
#29870=CARTESIAN_POINT('Origin',(-0.00570191777865816,-0.01700000000001,
0.0115714361099103));
#29871=CARTESIAN_POINT('Origin',(-0.0072568597527597,-0.01,0.0106652701104462));
#29872=CARTESIAN_POINT('',(-0.00766471363969575,-0.0225,0.0103760380117588));
#29873=CARTESIAN_POINT('',(-0.00766471363969575,-0.017,0.0103760380117588));
#29874=CARTESIAN_POINT('',(-0.00766471363970765,-0.01000000000001,0.0103760380117664));
#29875=CARTESIAN_POINT('',(-0.0068381037869931,-0.0225,0.0109384796291949));
#29876=CARTESIAN_POINT('Origin',(-0.00725685975277159,-0.02250000000001,
0.0106652701104539));
#29877=CARTESIAN_POINT('',(-0.0068381037869931,-0.017,0.0109384796291949));
#29878=CARTESIAN_POINT('',(-0.00683810378700499,-0.01000000000001,0.0109384796292026));
#29879=CARTESIAN_POINT('Origin',(-0.00725685975277159,-0.01700000000001,
0.0106652701104539));
#29880=CARTESIAN_POINT('Origin',(-0.00867055520634127,-0.01,0.00955151675985495));
#29881=CARTESIAN_POINT('',(-0.00903418655921466,-0.0225,0.00920833715788611));
#29882=CARTESIAN_POINT('',(-0.00903418655921466,-0.017,0.00920833715788611));
#29883=CARTESIAN_POINT('',(-0.00903418655922655,-0.01000000000001,0.00920833715789376));
#29884=CARTESIAN_POINT('',(-0.00829389796078363,-0.0225,0.00988034698864926));
#29885=CARTESIAN_POINT('Origin',(-0.00867055520635317,-0.02250000000001,
0.0095515167598626));
#29886=CARTESIAN_POINT('',(-0.00829389796078364,-0.017,0.00988034698864926));
#29887=CARTESIAN_POINT('',(-0.00829389796079552,-0.01000000000001,0.00988034698865692));
#29888=CARTESIAN_POINT('Origin',(-0.00867055520635317,-0.01700000000001,
0.0095515167598626));
#29889=CARTESIAN_POINT('Origin',(-0.00991548816544177,-0.01,0.0082518540002223));
#29890=CARTESIAN_POINT('',(-0.0102278193135934,-0.0225,0.00786140649556348));
#29891=CARTESIAN_POINT('',(-0.0102278193135934,-0.017,0.00786140649556348));
#29892=CARTESIAN_POINT('',(-0.0102278193136052,-0.01000000000001,0.00786140649557114));
#29893=CARTESIAN_POINT('',(-0.00958826084493661,-0.0225,0.0086299046326977));
#29894=CARTESIAN_POINT('Origin',(-0.00991548816545366,-0.02250000000001,
0.00825185400022996));
#29895=CARTESIAN_POINT('',(-0.00958826084493661,-0.017,0.0086299046326977));
#29896=CARTESIAN_POINT('',(-0.0095882608449485,-0.01000000000001,0.00862990463270536));
#29897=CARTESIAN_POINT('Origin',(-0.00991548816545366,-0.01700000000001,
0.00825185400022996));
#29898=CARTESIAN_POINT('Origin',(-0.0109674274261026,-0.01,0.0067915782888202));
#29899=CARTESIAN_POINT('',(-0.011222379199005,-0.0225,0.00636146249802205));
#29900=CARTESIAN_POINT('',(-0.011222379199005,-0.017,0.00636146249802205));
#29901=CARTESIAN_POINT('',(-0.0112223791990169,-0.01000000000001,0.00636146249802971));
#29902=CARTESIAN_POINT('',(-0.010695999138228,-0.0225,0.00721149099944164));
#29903=CARTESIAN_POINT('Origin',(-0.0109674274261145,-0.02250000000001,
0.00679157828882786));
#29904=CARTESIAN_POINT('',(-0.010695999138228,-0.017,0.00721149099944164));
#29905=CARTESIAN_POINT('',(-0.0106959991382398,-0.01000000000001,0.0072114909994493));
#29906=CARTESIAN_POINT('Origin',(-0.0109674274261145,-0.01700000000001,
0.00679157828882786));
#29907=CARTESIAN_POINT('Origin',(-0.0118058981871781,-0.01,0.005199112231332));
#29908=CARTESIAN_POINT('',(-0.0119985082385752,-0.0225,0.00473769986901296));
#29909=CARTESIAN_POINT('',(-0.0119985082385752,-0.017,0.00473769986901296));
#29910=CARTESIAN_POINT('',(-0.0119985082385871,-0.01000000000001,0.00473769986902062));
#29911=CARTESIAN_POINT('',(-0.0115955519748124,-0.0225,0.00565271389683093));
#29912=CARTESIAN_POINT('Origin',(-0.01180589818719,-0.02250000000001,0.00519911223133965));
#29913=CARTESIAN_POINT('',(-0.0115955519748124,-0.017,0.00565271389683093));
#29914=CARTESIAN_POINT('',(-0.0115955519748243,-0.01000000000001,0.00565271389683858));
#29915=CARTESIAN_POINT('Origin',(-0.01180589818719,-0.01700000000001,0.00519911223133965));
#29916=CARTESIAN_POINT('Origin',(-0.0124145805690504,-0.01,0.00350545136816342));
#29917=CARTESIAN_POINT('',(-0.0125410999633822,-0.0225,0.00302172330110727));
#29918=CARTESIAN_POINT('',(-0.0125410999633822,-0.017,0.00302172330110727));
#29919=CARTESIAN_POINT('',(-0.0125410999633941,-0.01000000000001,0.00302172330111493));
#29920=CARTESIAN_POINT('',(-0.012269410581952,-0.0225,0.00398391314808515));
#29921=CARTESIAN_POINT('Origin',(-0.0124145805690623,-0.02250000000001,
0.00350545136817107));
#29922=CARTESIAN_POINT('',(-0.012269410581952,-0.017,0.00398391314808515));
#29923=CARTESIAN_POINT('',(-0.0122694105819639,-0.01000000000001,0.00398391314809281));
#29924=CARTESIAN_POINT('Origin',(-0.0124145805690623,-0.01700000000001,
0.00350545136817107));
#29925=CARTESIAN_POINT('Origin',(-0.0127816272615221,-0.01,0.0017435608815054));
#29926=CARTESIAN_POINT('',(-0.0128395934426919,-0.0225,0.00124693232630483));
#29927=CARTESIAN_POINT('',(-0.0128395934426919,-0.017,0.00124693232630483));
#29928=CARTESIAN_POINT('',(-0.0128395934427038,-0.01000000000001,0.00124693232631249));
#29929=CARTESIAN_POINT('',(-0.0127044590683616,-0.0225,0.00223757006154593));
#29930=CARTESIAN_POINT('Origin',(-0.012781627261534,-0.02250000000001,0.00174356088151305));
#29931=CARTESIAN_POINT('',(-0.0127044590683616,-0.017,0.00223757006154593));
#29932=CARTESIAN_POINT('',(-0.0127044590683735,-0.01000000000001,0.00223757006155359));
#29933=CARTESIAN_POINT('Origin',(-0.012781627261534,-0.01700000000001,0.00174356088151305));
#29934=CARTESIAN_POINT('Origin',(-0.0128998941182339,-0.01,-5.22660344400411E-5));
#29935=CARTESIAN_POINT('',(-0.0128881788404607,-0.0225,-0.000552128767864633));
#29936=CARTESIAN_POINT('',(-0.0128881788404607,-0.017,-0.000552128767864633));
#29937=CARTESIAN_POINT('',(-0.0128881788404726,-0.01000000000001,-0.000552128767856978));
#29938=CARTESIAN_POINT('',(-0.0128922297101135,-0.0225,0.00044767521895696));
#29939=CARTESIAN_POINT('Origin',(-0.0128998941182458,-0.02250000000001,
-5.22660344323867E-5));
#29940=CARTESIAN_POINT('',(-0.0128922297101135,-0.017,0.00044767521895696));
#29941=CARTESIAN_POINT('',(-0.0128922297101254,-0.01000000000001,0.000447675218964614));
#29942=CARTESIAN_POINT('Origin',(-0.0128998941182458,-0.01700000000001,
-5.22660344323867E-5));
#29943=CARTESIAN_POINT('Origin',(-0.0127670792093463,-0.01,-0.00184707565147683));
#29944=CARTESIAN_POINT('',(-0.012685910497186,-0.0225,-0.00234044330360477));
#29945=CARTESIAN_POINT('',(-0.012685910497186,-0.017,-0.00234044330360477));
#29946=CARTESIAN_POINT('',(-0.0126859104971979,-0.01000000000001,-0.00234044330359712));
#29947=CARTESIAN_POINT('',(-0.012829067765252,-0.0225,-0.001350933112546));
#29948=CARTESIAN_POINT('Origin',(-0.0127670792093582,-0.02250000000001,
-0.00184707565146918));
#29949=CARTESIAN_POINT('',(-0.012829067765252,-0.017,-0.001350933112546));
#29950=CARTESIAN_POINT('',(-0.0128290677652638,-0.01000000000001,-0.00135093311253835));
#29951=CARTESIAN_POINT('Origin',(-0.0127670792093582,-0.01700000000001,
-0.00184707565146918));
#29952=CARTESIAN_POINT('Origin',(-0.0123857676259861,-0.01,-0.00360593404197504));
#29953=CARTESIAN_POINT('',(-0.0122367253360928,-0.0225,-0.00408320377265504));
#29954=CARTESIAN_POINT('',(-0.0122367253360928,-0.017,-0.00408320377265504));
#29955=CARTESIAN_POINT('',(-0.0122367253361005,-0.01000000000001,-0.00408320377266693));
#29956=CARTESIAN_POINT('',(-0.0125162026091882,-0.0225,-0.00312324706767692));
#29957=CARTESIAN_POINT('Origin',(-0.0123857676259938,-0.02250000000001,
-0.00360593404198693));
#29958=CARTESIAN_POINT('',(-0.0125162026091882,-0.017,-0.00312324706767692));
#29959=CARTESIAN_POINT('',(-0.0125162026091958,-0.01000000000001,-0.00312324706768881));
#29960=CARTESIAN_POINT('Origin',(-0.0123857676259938,-0.01700000000001,
-0.00360593404198693));
#29961=CARTESIAN_POINT('Origin',(-0.011763381164388,-0.01,-0.00529460702803539));
#29962=CARTESIAN_POINT('',(-0.0115493662354015,-0.0225,-0.00574648932484605));
#29963=CARTESIAN_POINT('',(-0.0115493662354015,-0.017,-0.00574648932484605));
#29964=CARTESIAN_POINT('',(-0.0115493662354091,-0.01000000000001,-0.00574648932485794));
#29965=CARTESIAN_POINT('',(-0.011959723806306,-0.0225,-0.00483477057127637));
#29966=CARTESIAN_POINT('Origin',(-0.0117633811643957,-0.02250000000001,
-0.00529460702804728));
#29967=CARTESIAN_POINT('',(-0.011959723806306,-0.017,-0.00483477057127637));
#29968=CARTESIAN_POINT('',(-0.0119597238063136,-0.01000000000001,-0.00483477057128826));
#29969=CARTESIAN_POINT('Origin',(-0.0117633811643957,-0.01700000000001,
-0.00529460702804728));
#29970=CARTESIAN_POINT('Origin',(-0.0109120338690729,-0.01,-0.00688022651082125));
#29971=CARTESIAN_POINT('',(-0.0106372118581474,-0.0225,-0.00729792599886364));
#29972=CARTESIAN_POINT('',(-0.0106372118581474,-0.017,-0.00729792599886364));
#29973=CARTESIAN_POINT('',(-0.010637211858155,-0.01000000000001,-0.00729792599887552));
#29974=CARTESIAN_POINT('',(-0.0111704625835182,-0.0225,-0.00645219076517593));
#29975=CARTESIAN_POINT('Origin',(-0.0109120338690805,-0.02250000000001,
-0.00688022651083314));
#29976=CARTESIAN_POINT('',(-0.0111704625835182,-0.017,-0.00645219076517593));
#29977=CARTESIAN_POINT('',(-0.0111704625835258,-0.01000000000001,-0.00645219076518782));
#29978=CARTESIAN_POINT('Origin',(-0.0109120338690805,-0.01700000000001,
-0.00688022651083314));
#29979=CARTESIAN_POINT('Origin',(-0.0098482962467508,-0.01,-0.00833193021071565));
#29980=CARTESIAN_POINT('',(-0.0095180162517236,-0.0225,-0.00870731684458113));
#29981=CARTESIAN_POINT('',(-0.0095180162517236,-0.017,-0.00870731684458113));
#29982=CARTESIAN_POINT('',(-0.00951801625173126,-0.01000000000001,-0.00870731684459302));
#29983=CARTESIAN_POINT('',(-0.0101637810127551,-0.0225,-0.00794402640508956));
#29984=CARTESIAN_POINT('Origin',(-0.00984829624675845,-0.02250000000001,
-0.00833193021072754));
#29985=CARTESIAN_POINT('',(-0.0101637810127551,-0.017,-0.00794402640508956));
#29986=CARTESIAN_POINT('',(-0.0101637810127627,-0.01000000000001,-0.00794402640510145));
#29987=CARTESIAN_POINT('Origin',(-0.00984829624675845,-0.01700000000001,
-0.00833193021072754));
#29988=CARTESIAN_POINT('Origin',(-0.00859287274025656,-0.01,-0.00962146236648858));
#29989=CARTESIAN_POINT('',(-0.00821356328554307,-0.0225,-0.00994722967234497));
#29990=CARTESIAN_POINT('',(-0.00821356328554307,-0.017,-0.00994722967234497));
#29991=CARTESIAN_POINT('',(-0.00821356328555072,-0.01000000000001,-0.00994722967235687));
#29992=CARTESIAN_POINT('',(-0.00895927300570829,-0.0225,-0.00928124060722424));
#29993=CARTESIAN_POINT('Origin',(-0.00859287274026421,-0.02250000000001,
-0.00962146236650047));
#29994=CARTESIAN_POINT('',(-0.00895927300570829,-0.017,-0.00928124060722424));
#29995=CARTESIAN_POINT('',(-0.00895927300571595,-0.01000000000001,-0.00928124060723613));
#29996=CARTESIAN_POINT('Origin',(-0.00859287274026421,-0.01700000000001,
-0.00962146236650047));
#29997=CARTESIAN_POINT('Origin',(-0.00717019874012118,-0.01,-0.0107237237015491));
#29998=CARTESIAN_POINT('',(-0.00674924265279915,-0.0225,-0.0109935309893427));
#29999=CARTESIAN_POINT('',(-0.00674924265279915,-0.017,-0.0109935309893427));
#30000=CARTESIAN_POINT('',(-0.00674924265280681,-0.01000000000001,-0.0109935309893545));
#30001=CARTESIAN_POINT('',(-0.00758038294062733,-0.0225,-0.010437806018194));
#30002=CARTESIAN_POINT('Origin',(-0.00717019874012884,-0.02250000000001,
-0.010723723701561));
#30003=CARTESIAN_POINT('',(-0.00758038294062733,-0.017,-0.010437806018194));
#30004=CARTESIAN_POINT('',(-0.00758038294063499,-0.01000000000001,-0.0104378060182059));
#30005=CARTESIAN_POINT('Origin',(-0.00717019874012884,-0.01700000000001,
-0.010723723701561));
#30006=CARTESIAN_POINT('Origin',(-0.00560796497748951,-0.01,-0.0116172599528138));
#30007=CARTESIAN_POINT('',(-0.00515355568896825,-0.0225,-0.011825855730589));
#30008=CARTESIAN_POINT('',(-0.00515355568896825,-0.017,-0.011825855730589));
#30009=CARTESIAN_POINT('',(-0.0051535556889759,-0.01000000000001,-0.0118258557306009));
#30010=CARTESIAN_POINT('',(-0.00605394934416489,-0.0225,-0.011391211407848));
#30011=CARTESIAN_POINT('Origin',(-0.00560796497749716,-0.02250000000001,
-0.0116172599528257));
#30012=CARTESIAN_POINT('',(-0.00605394934416489,-0.017,-0.011391211407848));
#30013=CARTESIAN_POINT('',(-0.00605394934417254,-0.01000000000001,-0.0113912114078599));
#30014=CARTESIAN_POINT('Origin',(-0.00560796497749716,-0.01700000000001,
-0.0116172599528257));
#30015=CARTESIAN_POINT('Origin',(-0.00393657855553661,-0.01,-0.0122846794535344));
#30016=CARTESIAN_POINT('',(-0.00345756062573429,-0.0225,-0.0124280036417509));
#30017=CARTESIAN_POINT('',(-0.00345756062573429,-0.017,-0.0124280036417509));
#30018=CARTESIAN_POINT('',(-0.00345756062574195,-0.01000000000001,-0.0124280036417628));
#30019=CARTESIAN_POINT('',(-0.00440968250998358,-0.0225,-0.0121228998247591));
#30020=CARTESIAN_POINT('Origin',(-0.00393657855554426,-0.02250000000001,
-0.0122846794535463));
#30021=CARTESIAN_POINT('',(-0.00440968250998358,-0.017,-0.0121228998247591));
#30022=CARTESIAN_POINT('',(-0.00440968250999122,-0.01000000000001,-0.012122899824771));
#30023=CARTESIAN_POINT('Origin',(-0.00393657855554426,-0.01700000000001,
-0.0122846794535463));
#30024=CARTESIAN_POINT('Origin',(-0.00218857110979193,-0.01,-0.0127129916423077));
#30025=CARTESIAN_POINT('',(-0.00169426807783735,-0.0225,-0.0127882545986707));
#30026=CARTESIAN_POINT('',(-0.00169426807783735,-0.017,-0.0127882545986707));
#30027=CARTESIAN_POINT('',(-0.00169426807784501,-0.01000000000001,-0.0127882545986826));
#30028=CARTESIAN_POINT('',(-0.00267958622168495,-0.0225,-0.0126186297861756));
#30029=CARTESIAN_POINT('Origin',(-0.00218857110979959,-0.02250000000001,
-0.0127129916423196));
#30030=CARTESIAN_POINT('',(-0.00267958622168495,-0.017,-0.0126186297861756));
#30031=CARTESIAN_POINT('',(-0.0026795862216926,-0.01000000000001,-0.0126186297861875));
#30032=CARTESIAN_POINT('Origin',(-0.00218857110979959,-0.01700000000001,
-0.0127129916423196));
#30033=CARTESIAN_POINT('Origin',(-0.000397965616857901,-0.01,-0.0128938599095771));
#30034=CARTESIAN_POINT('',(0.000102001470993324,-0.0225,-0.0128995967262514));
#30035=CARTESIAN_POINT('',(0.000102001470993324,-0.017,-0.0128995967262514));
#30036=CARTESIAN_POINT('',(0.000102001470985668,-0.01000000000001,-0.0128995967262633));
#30037=CARTESIAN_POINT('',(-0.000897334835565392,-0.0225,-0.0128687524722826));
#30038=CARTESIAN_POINT('Origin',(-0.000397965616865555,-0.02250000000001,
-0.012893859909589));
#30039=CARTESIAN_POINT('',(-0.000897334835565393,-0.017,-0.0128687524722826));
#30040=CARTESIAN_POINT('',(-0.000897334835573037,-0.01000000000001,-0.0128687524722945));
#30041=CARTESIAN_POINT('Origin',(-0.000397965616865556,-0.01700000000001,
-0.012893859909589));
#30042=CARTESIAN_POINT('Origin',(0.00140038582412907,-0.01,-0.0128237638602548));
#30043=CARTESIAN_POINT('',(0.00189628567721606,-0.0225,-0.0127598628766294));
#30044=CARTESIAN_POINT('',(0.00189628567721606,-0.017,-0.0127598628766294));
#30045=CARTESIAN_POINT('',(0.0018962856772084,-0.01000000000001,-0.0127598628766413));
#30046=CARTESIAN_POINT('',(0.000902382152425214,-0.0225,-0.0128683995295057));
#30047=CARTESIAN_POINT('Origin',(0.00140038582412142,-0.02250000000001,
-0.0128237638602667));
#30048=CARTESIAN_POINT('',(0.000902382152425214,-0.017,-0.0128683995295057));
#30049=CARTESIAN_POINT('',(0.000902382152417559,-0.01000000000001,-0.0128683995295176));
#30050=CARTESIAN_POINT('Origin',(0.00140038582412142,-0.01700000000001,
-0.0128237638602667));
#30051=CARTESIAN_POINT('Origin',(0.00317148034796465,-0.01,-0.0125040678342079));
#30052=CARTESIAN_POINT('',(0.0036536608397248,-0.0225,-0.0123717728102428));
#30053=CARTESIAN_POINT('',(0.0036536608397248,-0.017,-0.0123717728102428));
#30054=CARTESIAN_POINT('',(0.00365366083973669,-0.01000000000001,-0.0123717728102504));
#30055=CARTESIAN_POINT('',(0.00268453529826336,-0.0225,-0.0126175778274746));
#30056=CARTESIAN_POINT('Origin',(0.00317148034797655,-0.02250000000001,
-0.0125040678342156));
#30057=CARTESIAN_POINT('',(0.00268453529826336,-0.017,-0.0126175778274746));
#30058=CARTESIAN_POINT('',(0.0026845352982557,-0.01000000000001,-0.0126175778274865));
#30059=CARTESIAN_POINT('Origin',(0.00317148034797655,-0.01700000000001,
-0.0125040678342156));
#30060=CARTESIAN_POINT('Origin',(0.00488084561433254,-0.01,-0.0119409943509345));
#30061=CARTESIAN_POINT('',(0.00533992164996588,-0.0225,-0.0117428802587877));
#30062=CARTESIAN_POINT('',(0.00533992164996587,-0.017,-0.0117428802587877));
#30063=CARTESIAN_POINT('',(0.00533992164997777,-0.01000000000001,-0.0117428802587953));
#30064=CARTESIAN_POINT('',(0.00441443701813444,-0.0225,-0.0121211693253137));
#30065=CARTESIAN_POINT('Origin',(0.00488084561434443,-0.02250000000001,
-0.0119409943509422));
#30066=CARTESIAN_POINT('',(0.00441443701813444,-0.017,-0.0121211693253137));
#30067=CARTESIAN_POINT('',(0.00441443701814632,-0.01000000000001,-0.0121211693253213));
#30068=CARTESIAN_POINT('Origin',(0.00488084561434443,-0.01700000000001,
-0.0119409943509422));
#30069=CARTESIAN_POINT('Origin',(0.00649521077269703,-0.01,-0.0111455029953));
#30070=CARTESIAN_POINT('',(0.00692224695936122,-0.0225,-0.0108854259004236));
#30071=CARTESIAN_POINT('',(0.00692224695936122,-0.017,-0.0108854259004236));
#30072=CARTESIAN_POINT('',(0.00692224695937311,-0.01000000000001,-0.0108854259004312));
#30073=CARTESIAN_POINT('',(0.00605841674279519,-0.0225,-0.0113888360498612));
#30074=CARTESIAN_POINT('Origin',(0.00649521077270892,-0.02250000000001,
-0.0111455029953076));
#30075=CARTESIAN_POINT('',(0.00605841674279519,-0.017,-0.0113888360498612));
#30076=CARTESIAN_POINT('',(0.00605841674280708,-0.01000000000001,-0.0113888360498688));
#30077=CARTESIAN_POINT('Origin',(0.00649521077270892,-0.01700000000001,
-0.0111455029953076));
#30078=CARTESIAN_POINT('Origin',(0.00798315404156373,-0.01,-0.0101330771016836));
#30079=CARTESIAN_POINT('',(0.00836983860563182,-0.0225,-0.0098160991088963));
#30080=CARTESIAN_POINT('',(0.00836983860563182,-0.017,-0.0098160991088963));
#30081=CARTESIAN_POINT('',(0.00836983860564371,-0.01000000000001,-0.00981609910890396));
#30082=CARTESIAN_POINT('',(0.00758447627690437,-0.0225,-0.0104348320353073));
#30083=CARTESIAN_POINT('Origin',(0.00798315404157562,-0.02250000000001,
-0.0101330771016913));
#30084=CARTESIAN_POINT('',(0.00758447627690437,-0.017,-0.0104348320353073));
#30085=CARTESIAN_POINT('',(0.00758447627691626,-0.01000000000001,-0.0104348320353149));
#30086=CARTESIAN_POINT('Origin',(0.00798315404157562,-0.01700000000001,
-0.0101330771016913));
#30087=CARTESIAN_POINT('Origin',(0.00931571429771449,-0.01,-0.00892342238848729));
#30088=CARTESIAN_POINT('',(0.00965452086399409,-0.0225,-0.00855571311386156));
#30089=CARTESIAN_POINT('',(0.00965452086399409,-0.017,-0.00855571311386156));
#30090=CARTESIAN_POINT('',(0.00965452086400598,-0.01000000000001,-0.00855571311386922));
#30091=CARTESIAN_POINT('',(0.00896291260749749,-0.0225,-0.00927772588463158));
#30092=CARTESIAN_POINT('Origin',(0.00931571429772638,-0.02250000000001,
-0.00892342238849495));
#30093=CARTESIAN_POINT('',(0.00896291260749749,-0.017,-0.00927772588463158));
#30094=CARTESIAN_POINT('',(0.00896291260750938,-0.01000000000001,-0.00927772588463924));
#30095=CARTESIAN_POINT('Origin',(0.00931571429772638,-0.01700000000001,
-0.00892342238849495));
#30096=CARTESIAN_POINT('Origin',(0.0104669547715282,-0.01,-0.00754008340874168));
#30097=CARTESIAN_POINT('',(0.0107512888555934,-0.0225,-0.00712879989504486));
#30098=CARTESIAN_POINT('',(0.0107512888555934,-0.017,-0.00712879989504486));
#30099=CARTESIAN_POINT('',(0.0107512888556053,-0.01000000000001,-0.00712879989505252));
#30100=CARTESIAN_POINT('',(0.0101668960393476,-0.0225,-0.00794003935286826));
#30101=CARTESIAN_POINT('Origin',(0.0104669547715401,-0.02250000000001,-0.00754008340874933));
#30102=CARTESIAN_POINT('',(0.0101668960393476,-0.017,-0.00794003935286826));
#30103=CARTESIAN_POINT('',(0.0101668960393595,-0.01000000000001,-0.00794003935287591));
#30104=CARTESIAN_POINT('Origin',(0.0104669547715401,-0.01700000000001,-0.00754008340874933));
#30105=CARTESIAN_POINT('Origin',(0.0114144678766987,-0.01,-0.00600998528216265));
#30106=CARTESIAN_POINT('',(0.0116387952390284,-0.0225,-0.00556313269516086));
#30107=CARTESIAN_POINT('',(0.0116387952390284,-0.017,-0.00556313269516086));
#30108=CARTESIAN_POINT('',(0.0116387952390403,-0.01000000000001,-0.00556313269516851));
#30109=CARTESIAN_POINT('',(0.0111729924044647,-0.0225,-0.00644780898676229));
#30110=CARTESIAN_POINT('Origin',(0.0114144678767106,-0.02250000000001,-0.0060099852821703));
#30111=CARTESIAN_POINT('',(0.0111729924044647,-0.017,-0.00644780898676229));
#30112=CARTESIAN_POINT('',(0.0111729924044766,-0.01000000000001,-0.00644780898676994));
#30113=CARTESIAN_POINT('Origin',(0.0114144678767106,-0.01700000000001,-0.0060099852821703));
#30114=CARTESIAN_POINT('Origin',(0.0121398113484141,-0.01,-0.00436290962832323));
#30115=CARTESIAN_POINT('',(0.0122997657120691,-0.0225,-0.00388918544533519));
#30116=CARTESIAN_POINT('',(0.0122997657120691,-0.017,-0.00388918544533519));
#30117=CARTESIAN_POINT('',(0.012299765712081,-0.01000000000001,-0.00388918544534284));
#30118=CARTESIAN_POINT('',(0.0119616191815194,-0.0225,-0.004830079353003));
#30119=CARTESIAN_POINT('Origin',(0.012139811348426,-0.02250000000001,-0.00436290962833088));
#30120=CARTESIAN_POINT('',(0.0119616191815194,-0.017,-0.004830079353003));
#30121=CARTESIAN_POINT('',(0.0119616191815313,-0.01000000000001,-0.00483007935301066));
#30122=CARTESIAN_POINT('Origin',(0.012139811348426,-0.01700000000001,-0.00436290962833088));
#30123=CARTESIAN_POINT('Origin',(0.0126288672010633,-0.01,-0.00263091490130466));
#30124=CARTESIAN_POINT('',(0.0127213352363006,-0.0225,-0.00213953962469893));
#30125=CARTESIAN_POINT('',(0.0127213352363006,-0.017,-0.00213953962469893));
#30126=CARTESIAN_POINT('',(0.0127213352363125,-0.01000000000001,-0.00213953962470658));
#30127=CARTESIAN_POINT('',(0.012517426647346,-0.0225,-0.00311833771877137));
#30128=CARTESIAN_POINT('Origin',(0.0126288672010752,-0.02250000000001,-0.00263091490131231));
#30129=CARTESIAN_POINT('',(0.012517426647346,-0.017,-0.00311833771877137));
#30130=CARTESIAN_POINT('',(0.0125174266473579,-0.01000000000001,-0.00311833771877902));
#30131=CARTESIAN_POINT('Origin',(0.0126288672010752,-0.01700000000001,-0.00263091490131231));
#30132=CARTESIAN_POINT('Origin',(0.0128721165187673,-0.01,-0.000847712408353549));
#30133=CARTESIAN_POINT('',(0.0128952984404617,-0.0225,-0.000348250098958184));
#30134=CARTESIAN_POINT('',(0.0128952984404617,-0.017,-0.000348250098958184));
#30135=CARTESIAN_POINT('',(0.0128952984404736,-0.01000000000001,-0.000348250098965837));
#30136=CARTESIAN_POINT('',(0.0128295966418437,-0.0225,-0.00134590118790042));
#30137=CARTESIAN_POINT('Origin',(0.0128721165187792,-0.02250000000001,-0.000847712408361203));
#30138=CARTESIAN_POINT('',(0.0128295966418437,-0.017,-0.00134590118790042));
#30139=CARTESIAN_POINT('',(0.0128295966418555,-0.01000000000001,-0.00134590118790808));
#30140=CARTESIAN_POINT('Origin',(0.0128721165187792,-0.01700000000001,-0.000847712408361203));
#30141=CARTESIAN_POINT('Origin',(0.0128648247302491,-0.01,0.000951989842367618));
#30142=CARTESIAN_POINT('',(0.0128182693286638,-0.0225,0.00144981771883018));
#30143=CARTESIAN_POINT('',(0.0128182693286638,-0.017,0.00144981771883018));
#30144=CARTESIAN_POINT('',(0.0128182693286757,-0.01000000000001,0.00144981771882252));
#30145=CARTESIAN_POINT('',(0.0128920531311578,-0.0225,0.000452731778653103));
#30146=CARTESIAN_POINT('Origin',(0.012864824730261,-0.02250000000001,0.000951989842359964));
#30147=CARTESIAN_POINT('',(0.0128920531311578,-0.017,0.000452731778653103));
#30148=CARTESIAN_POINT('',(0.0128920531311697,-0.01000000000001,0.000452731778645449));
#30149=CARTESIAN_POINT('Origin',(0.012864824730261,-0.01700000000001,0.000951989842359964));
#30150=CARTESIAN_POINT('Origin',(-4.42567805516485E-17,-0.017,1.23897393496637E-32));
#30151=CARTESIAN_POINT('',(0.0124917471849488,-0.017,0.00321966648386474));
#30152=CARTESIAN_POINT('Origin',(-4.42567805516478E-17,-0.01700000000001,
1.23897393496654E-32));
#30153=CARTESIAN_POINT('',(0.0127035804707671,-0.017,0.00224255283610991));
#30154=CARTESIAN_POINT('Origin',(0.0126071337618875,-0.01700000000001,0.00273316269368159));
#30155=CARTESIAN_POINT('Origin',(-4.42567805516478E-17,-0.01700000000001,
1.23897393496654E-32));
#30156=CARTESIAN_POINT('Origin',(-4.42567805516478E-17,-0.01700000000001,
1.23897393496654E-32));
#30157=CARTESIAN_POINT('Origin',(-4.42567805516478E-17,-0.01700000000001,
1.23897393496654E-32));
#30158=CARTESIAN_POINT('Origin',(-4.42567805516478E-17,-0.01700000000001,
1.23897393496654E-32));
#30159=CARTESIAN_POINT('Origin',(-4.42567805516478E-17,-0.01700000000001,
1.23897393496654E-32));
#30160=CARTESIAN_POINT('Origin',(-4.42567805516478E-17,-0.01700000000001,
1.23897393496654E-32));
#30161=CARTESIAN_POINT('Origin',(-4.42567805516478E-17,-0.01700000000001,
1.23897393496654E-32));
#30162=CARTESIAN_POINT('Origin',(-4.42567805516478E-17,-0.01700000000001,
1.23897393496654E-32));
#30163=CARTESIAN_POINT('Origin',(-4.42567805516478E-17,-0.01700000000001,
1.23897393496654E-32));
#30164=CARTESIAN_POINT('Origin',(-4.42567805516478E-17,-0.01700000000001,
1.23897393496654E-32));
#30165=CARTESIAN_POINT('Origin',(-4.42567805516478E-17,-0.01700000000001,
1.23897393496654E-32));
#30166=CARTESIAN_POINT('Origin',(-4.42567805516478E-17,-0.01700000000001,
1.23897393496654E-32));
#30167=CARTESIAN_POINT('Origin',(-4.42567805516478E-17,-0.01700000000001,
1.23897393496654E-32));
#30168=CARTESIAN_POINT('Origin',(-4.42567805516478E-17,-0.01700000000001,
1.23897393496654E-32));
#30169=CARTESIAN_POINT('Origin',(-4.42567805516478E-17,-0.01700000000001,
1.23897393496654E-32));
#30170=CARTESIAN_POINT('Origin',(-4.42567805516478E-17,-0.01700000000001,
1.23897393496654E-32));
#30171=CARTESIAN_POINT('Origin',(-4.42567805516478E-17,-0.01700000000001,
1.23897393496654E-32));
#30172=CARTESIAN_POINT('Origin',(-4.42567805516478E-17,-0.01700000000001,
1.23897393496654E-32));
#30173=CARTESIAN_POINT('Origin',(-4.42567805516478E-17,-0.01700000000001,
1.23897393496654E-32));
#30174=CARTESIAN_POINT('Origin',(-4.42567805516478E-17,-0.01700000000001,
1.23897393496654E-32));
#30175=CARTESIAN_POINT('Origin',(-4.42567805516478E-17,-0.01700000000001,
1.23897393496654E-32));
#30176=CARTESIAN_POINT('Origin',(-4.42567805516478E-17,-0.01700000000001,
1.23897393496654E-32));
#30177=CARTESIAN_POINT('Origin',(-4.42567805516478E-17,-0.01700000000001,
1.23897393496654E-32));
#30178=CARTESIAN_POINT('Origin',(-4.42567805516478E-17,-0.01700000000001,
1.23897393496654E-32));
#30179=CARTESIAN_POINT('Origin',(-4.42567805516478E-17,-0.01700000000001,
1.23897393496654E-32));
#30180=CARTESIAN_POINT('Origin',(-4.42567805516478E-17,-0.01700000000001,
1.23897393496654E-32));
#30181=CARTESIAN_POINT('Origin',(-4.42567805516478E-17,-0.01700000000001,
1.23897393496654E-32));
#30182=CARTESIAN_POINT('Origin',(-4.42567805516478E-17,-0.01700000000001,
1.23897393496654E-32));
#30183=CARTESIAN_POINT('Origin',(-4.42567805516478E-17,-0.01700000000001,
1.23897393496654E-32));
#30184=CARTESIAN_POINT('Origin',(-4.42567805516478E-17,-0.01700000000001,
1.23897393496654E-32));
#30185=CARTESIAN_POINT('Origin',(-4.42567805516478E-17,-0.01700000000001,
1.23897393496654E-32));
#30186=CARTESIAN_POINT('Origin',(-4.42567805516478E-17,-0.01700000000001,
1.23897393496654E-32));
#30187=CARTESIAN_POINT('Origin',(-4.42567805516478E-17,-0.01700000000001,
1.23897393496654E-32));
#30188=CARTESIAN_POINT('Origin',(-4.42567805516478E-17,-0.01700000000001,
1.23897393496654E-32));
#30189=CARTESIAN_POINT('Origin',(-4.42567805516478E-17,-0.01700000000001,
1.23897393496654E-32));
#30190=CARTESIAN_POINT('Origin',(-4.42567805516478E-17,-0.01700000000001,
1.23897393496654E-32));
#30191=CARTESIAN_POINT('Origin',(-4.42567805516478E-17,-0.01700000000001,
1.23897393496654E-32));
#30192=CARTESIAN_POINT('Origin',(-4.42567805516478E-17,-0.01700000000001,
1.23897393496654E-32));
#30193=CARTESIAN_POINT('Origin',(-4.42567805516478E-17,-0.01700000000001,
1.23897393496654E-32));
#30194=CARTESIAN_POINT('Origin',(-4.42567805516478E-17,-0.01700000000001,
1.23897393496654E-32));
#30195=CARTESIAN_POINT('Origin',(-4.42567805516478E-17,-0.01700000000001,
1.23897393496654E-32));
#30196=CARTESIAN_POINT('Origin',(-4.42567805516478E-17,-0.01700000000001,
1.23897393496654E-32));
#30197=CARTESIAN_POINT('Origin',(-4.42567805516478E-17,-0.01700000000001,
1.23897393496654E-32));
#30198=CARTESIAN_POINT('Origin',(-4.42567805516478E-17,-0.01700000000001,
1.23897393496654E-32));
#30199=CARTESIAN_POINT('',(-0.000529682692573584,-0.01700000000001,0.0024432429771081));
#30200=CARTESIAN_POINT('Origin',(-4.42567805516478E-17,-0.01700000000001,
1.23897393496654E-32));
#30201=CARTESIAN_POINT('Origin',(-4.38905912375397E-17,-0.0225,1.33303635345025E-32));
#30202=CARTESIAN_POINT('',(0.0124917471849488,-0.0225,0.00321966648386474));
#30203=CARTESIAN_POINT('Origin',(-4.38905912375391E-17,-0.02250000000001,
1.33303635345042E-32));
#30204=CARTESIAN_POINT('',(0.0124917471849565,-0.01000000000001,0.00321966648387663));
#30205=CARTESIAN_POINT('Origin',(-4.38905912375397E-17,-0.0225,1.33303635345025E-32));
#30206=CARTESIAN_POINT('',(0.0127035804707671,-0.0225,0.00224255283610991));
#30207=CARTESIAN_POINT('',(0.012703580470779,-0.01000000000001,0.00224255283610226));
#30208=CARTESIAN_POINT('Origin',(-4.38905912375391E-17,-0.02250000000001,
1.33303635345042E-32));
#30209=CARTESIAN_POINT('Origin',(-4.38905912375397E-17,-0.0225,1.33303635345025E-32));
#30210=CARTESIAN_POINT('Origin',(-4.38905912375391E-17,-0.02250000000001,
1.33303635345042E-32));
#30211=CARTESIAN_POINT('Origin',(-4.38905912375397E-17,-0.0225,1.33303635345025E-32));
#30212=CARTESIAN_POINT('Origin',(-4.38905912375391E-17,-0.02250000000001,
1.33303635345042E-32));
#30213=CARTESIAN_POINT('Origin',(-4.38905912375397E-17,-0.0225,1.33303635345025E-32));
#30214=CARTESIAN_POINT('Origin',(-4.38905912375391E-17,-0.02250000000001,
1.33303635345042E-32));
#30215=CARTESIAN_POINT('Origin',(-4.38905912375397E-17,-0.0225,1.33303635345025E-32));
#30216=CARTESIAN_POINT('Origin',(-4.38905912375391E-17,-0.02250000000001,
1.33303635345042E-32));
#30217=CARTESIAN_POINT('Origin',(-4.38905912375397E-17,-0.0225,1.33303635345025E-32));
#30218=CARTESIAN_POINT('Origin',(-4.38905912375391E-17,-0.02250000000001,
1.33303635345042E-32));
#30219=CARTESIAN_POINT('Origin',(-4.38905912375397E-17,-0.0225,1.33303635345025E-32));
#30220=CARTESIAN_POINT('Origin',(-4.38905912375391E-17,-0.02250000000001,
1.33303635345042E-32));
#30221=CARTESIAN_POINT('Origin',(-4.38905912375397E-17,-0.0225,1.33303635345025E-32));
#30222=CARTESIAN_POINT('Origin',(-4.38905912375391E-17,-0.02250000000001,
1.33303635345042E-32));
#30223=CARTESIAN_POINT('Origin',(-4.38905912375397E-17,-0.0225,1.33303635345025E-32));
#30224=CARTESIAN_POINT('Origin',(-4.38905912375391E-17,-0.02250000000001,
1.33303635345042E-32));
#30225=CARTESIAN_POINT('Origin',(-4.38905912375397E-17,-0.0225,1.33303635345025E-32));
#30226=CARTESIAN_POINT('Origin',(-4.38905912375391E-17,-0.02250000000001,
1.33303635345042E-32));
#30227=CARTESIAN_POINT('Origin',(-4.38905912375397E-17,-0.0225,1.33303635345025E-32));
#30228=CARTESIAN_POINT('Origin',(-4.38905912375391E-17,-0.02250000000001,
1.33303635345042E-32));
#30229=CARTESIAN_POINT('Origin',(-4.38905912375397E-17,-0.0225,1.33303635345025E-32));
#30230=CARTESIAN_POINT('Origin',(-4.38905912375391E-17,-0.02250000000001,
1.33303635345042E-32));
#30231=CARTESIAN_POINT('Origin',(-4.38905912375397E-17,-0.0225,1.33303635345025E-32));
#30232=CARTESIAN_POINT('Origin',(-4.38905912375391E-17,-0.02250000000001,
1.33303635345042E-32));
#30233=CARTESIAN_POINT('Origin',(-4.38905912375397E-17,-0.0225,1.33303635345025E-32));
#30234=CARTESIAN_POINT('Origin',(-4.38905912375391E-17,-0.02250000000001,
1.33303635345042E-32));
#30235=CARTESIAN_POINT('Origin',(-4.38905912375397E-17,-0.0225,1.33303635345025E-32));
#30236=CARTESIAN_POINT('Origin',(-4.38905912375391E-17,-0.02250000000001,
1.33303635345042E-32));
#30237=CARTESIAN_POINT('Origin',(-4.38905912375397E-17,-0.0225,1.33303635345025E-32));
#30238=CARTESIAN_POINT('Origin',(-4.38905912375391E-17,-0.02250000000001,
1.33303635345042E-32));
#30239=CARTESIAN_POINT('Origin',(-4.38905912375397E-17,-0.0225,1.33303635345025E-32));
#30240=CARTESIAN_POINT('Origin',(-4.38905912375391E-17,-0.02250000000001,
1.33303635345042E-32));
#30241=CARTESIAN_POINT('Origin',(-4.38905912375397E-17,-0.0225,1.33303635345025E-32));
#30242=CARTESIAN_POINT('Origin',(-4.38905912375391E-17,-0.02250000000001,
1.33303635345042E-32));
#30243=CARTESIAN_POINT('Origin',(-4.38905912375397E-17,-0.0225,1.33303635345025E-32));
#30244=CARTESIAN_POINT('Origin',(-4.38905912375391E-17,-0.02250000000001,
1.33303635345042E-32));
#30245=CARTESIAN_POINT('Origin',(-4.38905912375397E-17,-0.0225,1.33303635345025E-32));
#30246=CARTESIAN_POINT('Origin',(-4.38905912375391E-17,-0.02250000000001,
1.33303635345042E-32));
#30247=CARTESIAN_POINT('Origin',(-4.38905912375397E-17,-0.0225,1.33303635345025E-32));
#30248=CARTESIAN_POINT('Origin',(-4.38905912375391E-17,-0.02250000000001,
1.33303635345042E-32));
#30249=CARTESIAN_POINT('Origin',(-4.38905912375397E-17,-0.0225,1.33303635345025E-32));
#30250=CARTESIAN_POINT('Origin',(-4.38905912375391E-17,-0.02250000000001,
1.33303635345042E-32));
#30251=CARTESIAN_POINT('Origin',(-4.38905912375397E-17,-0.0225,1.33303635345025E-32));
#30252=CARTESIAN_POINT('Origin',(-4.38905912375391E-17,-0.02250000000001,
1.33303635345042E-32));
#30253=CARTESIAN_POINT('Origin',(-4.38905912375397E-17,-0.0225,1.33303635345025E-32));
#30254=CARTESIAN_POINT('Origin',(-4.38905912375391E-17,-0.02250000000001,
1.33303635345042E-32));
#30255=CARTESIAN_POINT('Origin',(-4.38905912375397E-17,-0.0225,1.33303635345025E-32));
#30256=CARTESIAN_POINT('Origin',(-4.38905912375391E-17,-0.02250000000001,
1.33303635345042E-32));
#30257=CARTESIAN_POINT('Origin',(-4.38905912375397E-17,-0.0225,1.33303635345025E-32));
#30258=CARTESIAN_POINT('Origin',(-4.38905912375391E-17,-0.02250000000001,
1.33303635345042E-32));
#30259=CARTESIAN_POINT('Origin',(-4.38905912375397E-17,-0.0225,1.33303635345025E-32));
#30260=CARTESIAN_POINT('Origin',(-4.38905912375391E-17,-0.02250000000001,
1.33303635345042E-32));
#30261=CARTESIAN_POINT('Origin',(-4.38905912375397E-17,-0.0225,1.33303635345025E-32));
#30262=CARTESIAN_POINT('Origin',(-4.38905912375391E-17,-0.02250000000001,
1.33303635345042E-32));
#30263=CARTESIAN_POINT('Origin',(-4.38905912375397E-17,-0.0225,1.33303635345025E-32));
#30264=CARTESIAN_POINT('Origin',(-4.38905912375391E-17,-0.02250000000001,
1.33303635345042E-32));
#30265=CARTESIAN_POINT('Origin',(-4.38905912375397E-17,-0.0225,1.33303635345025E-32));
#30266=CARTESIAN_POINT('Origin',(-4.38905912375391E-17,-0.02250000000001,
1.33303635345042E-32));
#30267=CARTESIAN_POINT('Origin',(-4.38905912375397E-17,-0.0225,1.33303635345025E-32));
#30268=CARTESIAN_POINT('Origin',(-4.38905912375391E-17,-0.02250000000001,
1.33303635345042E-32));
#30269=CARTESIAN_POINT('Origin',(-4.38905912375397E-17,-0.0225,1.33303635345025E-32));
#30270=CARTESIAN_POINT('Origin',(-4.38905912375391E-17,-0.02250000000001,
1.33303635345042E-32));
#30271=CARTESIAN_POINT('Origin',(-4.38905912375397E-17,-0.0225,1.33303635345025E-32));
#30272=CARTESIAN_POINT('Origin',(-4.38905912375391E-17,-0.02250000000001,
1.33303635345042E-32));
#30273=CARTESIAN_POINT('Origin',(-4.38905912375397E-17,-0.0225,1.33303635345025E-32));
#30274=CARTESIAN_POINT('Origin',(-4.38905912375391E-17,-0.02250000000001,
1.33303635345042E-32));
#30275=CARTESIAN_POINT('Origin',(-4.38905912375397E-17,-0.0225,1.33303635345025E-32));
#30276=CARTESIAN_POINT('Origin',(-4.38905912375391E-17,-0.02250000000001,
1.33303635345042E-32));
#30277=CARTESIAN_POINT('Origin',(-4.38905912375397E-17,-0.0225,1.33303635345025E-32));
#30278=CARTESIAN_POINT('Origin',(-4.38905912375391E-17,-0.02250000000001,
1.33303635345042E-32));
#30279=CARTESIAN_POINT('Origin',(-4.38905912375397E-17,-0.0225,1.33303635345025E-32));
#30280=CARTESIAN_POINT('Origin',(-4.38905912375391E-17,-0.02250000000001,
1.33303635345042E-32));
#30281=CARTESIAN_POINT('Origin',(-4.38905912375397E-17,-0.0225,1.33303635345025E-32));
#30282=CARTESIAN_POINT('Origin',(-4.38905912375391E-17,-0.02250000000001,
1.33303635345042E-32));
#30283=CARTESIAN_POINT('Origin',(-4.38905912375397E-17,-0.0225,1.33303635345025E-32));
#30284=CARTESIAN_POINT('Origin',(-4.38905912375391E-17,-0.02250000000001,
1.33303635345042E-32));
#30285=CARTESIAN_POINT('Origin',(-4.38905912375397E-17,-0.0225,1.33303635345025E-32));
#30286=CARTESIAN_POINT('Origin',(-4.38905912375391E-17,-0.02250000000001,
1.33303635345042E-32));
#30287=CARTESIAN_POINT('Origin',(-4.38905912375397E-17,-0.0225,1.33303635345025E-32));
#30288=CARTESIAN_POINT('Origin',(-4.38905912375391E-17,-0.02250000000001,
1.33303635345042E-32));
#30289=CARTESIAN_POINT('Origin',(-4.38905912375397E-17,-0.0225,1.33303635345025E-32));
#30290=CARTESIAN_POINT('Origin',(-4.38905912375391E-17,-0.02250000000001,
1.33303635345042E-32));
#30291=CARTESIAN_POINT('Origin',(-4.38905912375397E-17,-0.0225,1.33303635345025E-32));
#30292=CARTESIAN_POINT('Origin',(-4.38905912375391E-17,-0.02250000000001,
1.33303635345042E-32));
#30293=CARTESIAN_POINT('Origin',(0.0126071337618777,-0.01,0.00273316269367947));
#30294=CARTESIAN_POINT('Origin',(0.0126071337618875,-0.02250000000001,0.00273316269368159));
#30295=CARTESIAN_POINT('Origin',(-4.38905912375397E-17,-0.0225,1.33303635345025E-32));
#30296=CARTESIAN_POINT('Origin',(-4.38905912375391E-17,-0.02250000000001,
1.33303635345042E-32));
#30297=CARTESIAN_POINT('',(-0.000529682692573584,-0.02250000000001,0.0024432429771081));
#30298=CARTESIAN_POINT('Origin',(-4.38905912375391E-17,-0.02250000000001,
1.33303635345042E-32));
#30299=CARTESIAN_POINT('Origin',(-4.38905912375397E-17,-0.0225,1.33303635345025E-32));
#30300=CARTESIAN_POINT('Origin',(-4.38905912375397E-17,-0.0225,1.33303635345025E-32));
#30301=CARTESIAN_POINT('',(-0.000529682692573584,-0.0225,0.0024432429771081));
#30302=CARTESIAN_POINT('',(0.,0.,0.));
#30303=CARTESIAN_POINT('Origin',(-0.0129631448730623,-0.024,0.02115));
#30304=CARTESIAN_POINT('',(0.0129631448730622,-0.0244065057546663,0.0211500000000126));
#30305=CARTESIAN_POINT('',(-0.0129631448730623,-0.0244065057553825,0.02115));
#30306=CARTESIAN_POINT('',(0.00151842756346932,-0.0244065057553835,0.02115));
#30307=CARTESIAN_POINT('',(0.0129631448730622,-0.024,0.0211500000000126));
#30308=CARTESIAN_POINT('',(0.0129631448730622,-0.024,0.0211500000000126));
#30309=CARTESIAN_POINT('',(-0.0129631448730623,-0.024,0.02115));
#30310=CARTESIAN_POINT('',(-0.00648157243653117,-0.024,0.02115));
#30311=CARTESIAN_POINT('',(-0.0129631448730623,-0.024,0.02115));
#30312=CARTESIAN_POINT('Origin',(-0.0129631448730724,-0.024,0.0191500000000103));
#30313=CARTESIAN_POINT('',(-0.0137123694637994,-0.0327500380762009,0.0210043631016193));
#30314=CARTESIAN_POINT('Origin',(-0.0129631448730724,-0.138986429016312,
0.0191500000000103));
#30315=CARTESIAN_POINT('',(-0.0140842817269636,-0.024,0.0208062162162381));
#30316=CARTESIAN_POINT('Origin',(-0.0129631448730724,-0.024,0.0191500000000103));
#30317=CARTESIAN_POINT('',(-0.0140842817269636,-0.0329447564781601,0.0208062162162381));
#30318=CARTESIAN_POINT('',(-0.0140842817269636,-0.024,0.0208062162162381));
#30319=CARTESIAN_POINT('Origin',(-0.0129631448730724,-0.034572315620975,
0.0191500000000103));
#30320=CARTESIAN_POINT('Origin',(-1.00275343584144E-14,-0.024,9.9475983006414E-15));
#30321=CARTESIAN_POINT('',(-0.0141669730359352,-0.033,0.02075000000001));
#30322=CARTESIAN_POINT('Origin',(-1.00275343584144E-14,-0.0533909682096408,
9.9475983006414E-15));
#30323=CARTESIAN_POINT('',(-0.0208062162162391,-0.024,0.0140842817269642));
#30324=CARTESIAN_POINT('Origin',(-1.00275343584144E-14,-0.024,9.9475983006414E-15));
#30325=CARTESIAN_POINT('',(-0.0208062162162391,-0.0329447564781591,0.0140842817269642));
#30326=CARTESIAN_POINT('',(-0.0208062162162391,-0.024,0.0140842817269642));
#30327=CARTESIAN_POINT('',(-0.0207500000000101,-0.033,0.014166973035935));
#30328=CARTESIAN_POINT('Origin',(-1.00275343584144E-14,-0.0533909682096407,
9.9475983006414E-15));
#30329=CARTESIAN_POINT('',(-0.0181707160081772,-0.033,0.017351965443474));
#30330=CARTESIAN_POINT('Origin',(-1.00275343584144E-14,-0.033,9.9475983006414E-15));
#30331=CARTESIAN_POINT('',(-0.017351965443474,-0.033,0.0181707160081772));
#30332=CARTESIAN_POINT('Ctrl Pts',(-0.0173519654434766,-0.0330000000000234,
0.0181707160081747));
#30333=CARTESIAN_POINT('Ctrl Pts',(-0.0175505715951354,-0.0329573203740106,
0.0179810588103573));
#30334=CARTESIAN_POINT('Ctrl Pts',(-0.017753450710576,-0.0329436053651554,
0.0177809667685882));
#30335=CARTESIAN_POINT('Ctrl Pts',(-0.0180265973873143,-0.0329719202135652,
0.0175019481550689));
#30336=CARTESIAN_POINT('Ctrl Pts',(-0.0180989364030346,-0.0329838470317312,
0.0174271319613231));
#30337=CARTESIAN_POINT('Ctrl Pts',(-0.0181707160081747,-0.0330000000000234,
0.0173519654434766));
#30338=CARTESIAN_POINT('Origin',(-1.00275343584144E-14,-0.033,9.9475983006414E-15));
#30339=CARTESIAN_POINT('Origin',(-0.0191500000000098,-0.024,0.0129631448730722));
#30340=CARTESIAN_POINT('',(-0.0210043631016193,-0.0327500380762009,0.0137123694638626));
#30341=CARTESIAN_POINT('Origin',(-0.0191500000000098,-0.0345723156209755,
0.0129631448730722));
#30342=CARTESIAN_POINT('',(-0.0211500000000238,-0.024,0.0129631448730623));
#30343=CARTESIAN_POINT('Origin',(-0.0191500000000098,-0.024,0.0129631448730722));
#30344=CARTESIAN_POINT('',(-0.0211500000000238,-0.0244065057540237,0.0129631448730623));
#30345=CARTESIAN_POINT('',(-0.0211500000000238,-0.024,0.0129631448730623));
#30346=CARTESIAN_POINT('Origin',(-0.0191500000000098,-0.138986429016342,
0.0129631448730722));
#30347=CARTESIAN_POINT('Origin',(-0.02115,-0.024,-0.0129631448730623));
#30348=CARTESIAN_POINT('',(-0.02115,-0.0244065057553841,-0.0129631448730623));
#30349=CARTESIAN_POINT('',(-0.02115,-0.0244065057553851,0.00151842756346924));
#30350=CARTESIAN_POINT('',(-0.02115,-0.024,-0.0129631448730623));
#30351=CARTESIAN_POINT('',(-0.02115,-0.024,-0.00648157243653115));
#30352=CARTESIAN_POINT('',(-0.02115,-0.024,-0.0129631448730623));
#30353=CARTESIAN_POINT('Origin',(-0.01915000000001,-0.024,-0.0129631448730723));
#30354=CARTESIAN_POINT('',(-0.0210043631016193,-0.0327500380762009,-0.0137123694637993));
#30355=CARTESIAN_POINT('Origin',(-0.01915000000001,-0.138986429016327,-0.0129631448730723));
#30356=CARTESIAN_POINT('',(-0.0208062162162194,-0.024,-0.0140842817269509));
#30357=CARTESIAN_POINT('Origin',(-0.01915000000001,-0.024,-0.0129631448730723));
#30358=CARTESIAN_POINT('',(-0.0208062162162194,-0.0329447564781784,-0.0140842817269509));
#30359=CARTESIAN_POINT('',(-0.0208062162162194,-0.024,-0.0140842817269509));
#30360=CARTESIAN_POINT('Origin',(-0.01915000000001,-0.0345723156209752,
-0.0129631448730723));
#30361=CARTESIAN_POINT('Origin',(-1.00275343584144E-14,-0.024,9.9475983006414E-15));
#30362=CARTESIAN_POINT('',(-0.0207500000000101,-0.033,-0.0141669730359174));
#30363=CARTESIAN_POINT('Origin',(-1.00275343584144E-14,-0.0533909682096407,
9.9475983006414E-15));
#30364=CARTESIAN_POINT('',(-0.014084281726955,-0.024,-0.0208062162162255));
#30365=CARTESIAN_POINT('Origin',(-1.00275343584144E-14,-0.024,9.9475983006414E-15));
#30366=CARTESIAN_POINT('',(-0.014084281726955,-0.0329447564781725,-0.0208062162162255));
#30367=CARTESIAN_POINT('',(-0.014084281726955,-0.024,-0.0208062162162255));
#30368=CARTESIAN_POINT('',(-0.0141669730359082,-0.033,-0.02075000000001));
#30369=CARTESIAN_POINT('Origin',(-1.00275343584144E-14,-0.0533909682096603,
9.9475983006414E-15));
#30370=CARTESIAN_POINT('',(-0.0173519654434044,-0.033,-0.0181707160082254));
#30371=CARTESIAN_POINT('Origin',(-1.00275343584144E-14,-0.033,9.9475983006414E-15));
#30372=CARTESIAN_POINT('',(-0.018170716008223,-0.033,-0.0173519654434079));
#30373=CARTESIAN_POINT('Ctrl Pts',(-0.0181707160082205,-0.0330000000000234,
-0.0173519654434105));
#30374=CARTESIAN_POINT('Ctrl Pts',(-0.0179810588103863,-0.0329573203740007,
-0.0175505715950879));
#30375=CARTESIAN_POINT('Ctrl Pts',(-0.0177809667685979,-0.0329436053651405,
-0.0177534507105486));
#30376=CARTESIAN_POINT('Ctrl Pts',(-0.0175019481550389,-0.0329719202135544,
-0.0180265973873254));
#30377=CARTESIAN_POINT('Ctrl Pts',(-0.0174271319612734,-0.0329838470317247,
-0.0180989364030644));
#30378=CARTESIAN_POINT('Ctrl Pts',(-0.0173519654434071,-0.0330000000000234,
-0.0181707160082229));
#30379=CARTESIAN_POINT('Origin',(-1.00275343584144E-14,-0.033,9.9475983006414E-15));
#30380=CARTESIAN_POINT('Origin',(-0.0129631448730721,-0.024,-0.0191500000000097));
#30381=CARTESIAN_POINT('',(-0.0137123694638186,-0.0327500380762009,-0.0210043631016193));
#30382=CARTESIAN_POINT('Origin',(-0.0129631448730721,-0.0345723156209755,
-0.0191500000000097));
#30383=CARTESIAN_POINT('',(-0.0129631448730622,-0.024,-0.0211500000000074));
#30384=CARTESIAN_POINT('Origin',(-0.0129631448730721,-0.024,-0.0191500000000097));
#30385=CARTESIAN_POINT('',(-0.0129631448730622,-0.0244065057549635,-0.0211500000000074));
#30386=CARTESIAN_POINT('',(-0.0129631448730622,-0.024,-0.0211500000000074));
#30387=CARTESIAN_POINT('Origin',(-0.0129631448730721,-0.138986429016347,
-0.0191500000000097));
#30388=CARTESIAN_POINT('Origin',(0.0129631448730622,-0.024,-0.0211500000000226));
#30389=CARTESIAN_POINT('',(0.0129631448730622,-0.0244065057540901,-0.0211500000000226));
#30390=CARTESIAN_POINT('',(-0.00151842756367382,-0.0244065057548141,-0.02115000000001));
#30391=CARTESIAN_POINT('',(0.0129631448730622,-0.024,-0.0211500000000226));
#30392=CARTESIAN_POINT('',(0.00648157243652186,-0.024,-0.0211500000000169));
#30393=CARTESIAN_POINT('',(0.0129631448730622,-0.024,-0.0211500000000226));
#30394=CARTESIAN_POINT('Origin',(0.012963144873072,-0.024,-0.0191500000000096));
#30395=CARTESIAN_POINT('',(0.0137123694638594,-0.0327500380762009,-0.0210043631016193));
#30396=CARTESIAN_POINT('Origin',(0.012963144873072,-0.138986429016351,-0.0191500000000096));
#30397=CARTESIAN_POINT('',(0.0140842817269635,-0.024,-0.0208062162162381));
#30398=CARTESIAN_POINT('Origin',(0.012963144873072,-0.024,-0.0191500000000096));
#30399=CARTESIAN_POINT('',(0.0140842817269635,-0.0329447564781601,-0.0208062162162381));
#30400=CARTESIAN_POINT('',(0.0140842817269635,-0.024,-0.0208062162162381));
#30401=CARTESIAN_POINT('Origin',(0.012963144873072,-0.0345723156209756,
-0.0191500000000096));
#30402=CARTESIAN_POINT('Origin',(-1.00275343584144E-14,-0.024,9.9475983006414E-15));
#30403=CARTESIAN_POINT('',(0.0141669730358882,-0.033,-0.02075000000001));
#30404=CARTESIAN_POINT('Origin',(-1.00275343584144E-14,-0.0533909682096603,
9.9475983006414E-15));
#30405=CARTESIAN_POINT('',(0.0208062162162161,-0.024,-0.0140842817269487));
#30406=CARTESIAN_POINT('Origin',(-1.00275343584144E-14,-0.024,9.9475983006414E-15));
#30407=CARTESIAN_POINT('',(0.0208062162162161,-0.0329447564781817,-0.0140842817269487));
#30408=CARTESIAN_POINT('',(0.0208062162162161,-0.024,-0.0140842817269487));
#30409=CARTESIAN_POINT('',(0.02075000000001,-0.033,-0.0141669730358881));
#30410=CARTESIAN_POINT('Origin',(-1.00275343584144E-14,-0.0533909682096601,
9.9475983006414E-15));
#30411=CARTESIAN_POINT('',(0.0181707160082761,-0.033,-0.0173519654433313));
#30412=CARTESIAN_POINT('Origin',(-1.00275343584144E-14,-0.033,9.9475983006414E-15));
#30413=CARTESIAN_POINT('',(0.0173519654433313,-0.033,-0.0181707160082761));
#30414=CARTESIAN_POINT('Ctrl Pts',(0.0173519654433339,-0.0330000000000234,
-0.0181707160082736));
#30415=CARTESIAN_POINT('Ctrl Pts',(0.0175505715950326,-0.0329573203739897,
-0.0179810588104207));
#30416=CARTESIAN_POINT('Ctrl Pts',(0.0177534507105162,-0.0329436053651239,
-0.0177809667686107));
#30417=CARTESIAN_POINT('Ctrl Pts',(0.0180265973873359,-0.0329719202135427,
-0.0175019481550082));
#30418=CARTESIAN_POINT('Ctrl Pts',(0.0180989364030953,-0.0329838470317177,
-0.0174271319612215));
#30419=CARTESIAN_POINT('Ctrl Pts',(0.0181707160082736,-0.0330000000000234,
-0.0173519654433339));
#30420=CARTESIAN_POINT('Origin',(-1.00275343584144E-14,-0.033,9.9475983006414E-15));
#30421=CARTESIAN_POINT('Origin',(0.0211500000000181,-0.024,-0.00793218971944487));
#30422=CARTESIAN_POINT('',(0.0211500000000181,-0.031,-0.00793218971944487));
#30423=CARTESIAN_POINT('',(0.0211500000000182,-0.03099999999999,-0.00800000000000997));
#30424=CARTESIAN_POINT('',(0.0211500000000147,-0.031,-0.00396609485971326));
#30425=CARTESIAN_POINT('',(0.0211500000000181,-0.0328178102805551,-0.00793218971944487));
#30426=CARTESIAN_POINT('',(0.0211500000000181,-0.024,-0.00793218971944487));
#30427=CARTESIAN_POINT('',(0.0211500000000182,-0.03274999999999,-0.00800000000000997));
#30428=CARTESIAN_POINT('',(0.02115000000002,-0.0306419525701411,-0.0101080474298589));
#30429=CARTESIAN_POINT('',(0.0211500000000182,-0.0283771628421106,-0.008));
#30430=CARTESIAN_POINT('Origin',(0.02115,-0.024,0.0129631448730622));
#30431=CARTESIAN_POINT('',(0.0211500000000043,-0.03099999999999,0.00800000000001003));
#30432=CARTESIAN_POINT('',(0.0211500000000044,-0.031,0.00793218971944469));
#30433=CARTESIAN_POINT('',(0.0211500000000056,-0.031,0.00648157243654025));
#30434=CARTESIAN_POINT('',(0.0211500000000043,-0.03274999999999,0.00800000000001004));
#30435=CARTESIAN_POINT('',(0.0211500000000043,-0.0285,0.008));
#30436=CARTESIAN_POINT('',(0.0211500000000044,-0.0328178102805553,0.00793218971944469));
#30437=CARTESIAN_POINT('',(0.0211500000000014,-0.0293842137817322,0.0113657862182679));
#30438=CARTESIAN_POINT('',(0.0211500000000044,-0.024,0.00793218971944469));
#30439=CARTESIAN_POINT('Origin',(0.0211500000000044,-0.024,0.00793218971944473));
#30440=CARTESIAN_POINT('',(0.0248178102805753,-0.03099999999999,0.00793218971944473));
#30441=CARTESIAN_POINT('',(0.0105750000000022,-0.031,0.00793218971944473));
#30442=CARTESIAN_POINT('',(0.02475000000001,-0.0328178102805653,0.00793218971944473));
#30443=CARTESIAN_POINT('',(0.0158250000000022,-0.0328178102805553,0.00793218971944473));
#30444=CARTESIAN_POINT('',(0.0248178102805753,-0.03274999999999,0.00793218971944473));
#30445=CARTESIAN_POINT('',(0.0261339051402787,-0.0314339051402766,0.00793218971944473));
#30446=CARTESIAN_POINT('',(0.0248178102805553,-0.0285,0.00793218971944473));
#30447=CARTESIAN_POINT('Origin',(0.02115,-0.024,0.0129631448730622));
#30448=CARTESIAN_POINT('',(0.0211500000000043,-0.0244065057561963,0.00800000000001003));
#30449=CARTESIAN_POINT('',(0.02115,-0.0244065057553837,0.0129631448730622));
#30450=CARTESIAN_POINT('',(0.0211500000000126,-0.0244065057546653,-0.00151842756326574));
#30451=CARTESIAN_POINT('',(0.0211500000000043,-0.02399999999999,0.00800000000000138));
#30452=CARTESIAN_POINT('',(0.0211500000000043,-0.024,0.008));
#30453=CARTESIAN_POINT('',(0.02115,-0.024,0.0129631448730622));
#30454=CARTESIAN_POINT('',(0.0211500000000056,-0.024,0.00648157243654025));
#30455=CARTESIAN_POINT('',(0.02115,-0.024,0.0129631448730622));
#30456=CARTESIAN_POINT('Origin',(0.01915000000001,-0.024,0.0129631448730722));
#30457=CARTESIAN_POINT('',(0.0210043631016192,-0.0327500380762009,0.0137123694637995));
#30458=CARTESIAN_POINT('',(0.020806216216238,-0.0329447564781601,0.0140842817269634));
#30459=CARTESIAN_POINT('Origin',(0.01915000000001,-0.0345723156209752,0.0129631448730722));
#30460=CARTESIAN_POINT('Origin',(0.01915000000001,-0.138986429016329,0.0129631448730722));
#30461=CARTESIAN_POINT('',(0.020806216216238,-0.024,0.0140842817269634));
#30462=CARTESIAN_POINT('Origin',(0.01915000000001,-0.024,0.0129631448730722));
#30463=CARTESIAN_POINT('',(0.020806216216238,-0.024,0.0140842817269634));
#30464=CARTESIAN_POINT('Origin',(-1.00275343584144E-14,-0.024,9.9475983006414E-15));
#30465=CARTESIAN_POINT('',(0.0141669730359443,-0.033,0.02075000000001));
#30466=CARTESIAN_POINT('',(0.014084281726958,-0.0329447564781683,0.0208062162162298));
#30467=CARTESIAN_POINT('Origin',(-1.00275343584144E-14,-0.0533909682096408,
9.9475983006414E-15));
#30468=CARTESIAN_POINT('',(0.017351965443488,-0.033,0.0181707160081675));
#30469=CARTESIAN_POINT('Origin',(-1.00275343584144E-14,-0.033,9.9475983006414E-15));
#30470=CARTESIAN_POINT('',(0.0181707160081698,-0.033,0.0173519654434845));
#30471=CARTESIAN_POINT('Ctrl Pts',(0.0181707160081673,-0.0330000000000234,
0.0173519654434871));
#30472=CARTESIAN_POINT('Ctrl Pts',(0.017981058810353,-0.0329573203740124,
0.0175505715951428));
#30473=CARTESIAN_POINT('Ctrl Pts',(0.0177809667685874,-0.0329436053651581,
0.0177534507105799));
#30474=CARTESIAN_POINT('Ctrl Pts',(0.0175019481550755,-0.0329719202135672,
0.0180265973873114));
#30475=CARTESIAN_POINT('Ctrl Pts',(0.0174271319613334,-0.0329838470317324,
0.0180989364030283));
#30476=CARTESIAN_POINT('Ctrl Pts',(0.0173519654434906,-0.0330000000000234,
0.0181707160081649));
#30477=CARTESIAN_POINT('',(0.02075000000001,-0.033,0.0141669730359351));
#30478=CARTESIAN_POINT('Origin',(-1.00275343584144E-14,-0.033,9.9475983006414E-15));
#30479=CARTESIAN_POINT('Origin',(-1.00275343584144E-14,-0.0533909682096601,
9.9475983006414E-15));
#30480=CARTESIAN_POINT('',(0.014084281726958,-0.024,0.0208062162162298));
#30481=CARTESIAN_POINT('Origin',(-1.00275343584144E-14,-0.024,9.9475983006414E-15));
#30482=CARTESIAN_POINT('',(0.014084281726958,-0.024,0.0208062162162298));
#30483=CARTESIAN_POINT('Origin',(0.0129631448730721,-0.024,0.0191500000000096));
#30484=CARTESIAN_POINT('',(0.0137123694638326,-0.0327500380762009,0.0210043631016193));
#30485=CARTESIAN_POINT('Origin',(0.0129631448730721,-0.138986429016353,
0.0191500000000096));
#30486=CARTESIAN_POINT('Origin',(0.0129631448730721,-0.0345723156209757,
0.0191500000000096));
#30487=CARTESIAN_POINT('Origin',(0.0129631448730721,-0.024,0.0191500000000096));
#30488=CARTESIAN_POINT('Origin',(0.01915000000001,-0.024,-0.0129631448730722));
#30489=CARTESIAN_POINT('',(0.0211500000000225,-0.024,-0.0129631448730622));
#30490=CARTESIAN_POINT('Origin',(0.01915000000001,-0.024,-0.0129631448730722));
#30491=CARTESIAN_POINT('',(0.0211500000000225,-0.0244065057540974,-0.0129631448730622));
#30492=CARTESIAN_POINT('',(0.0211500000000225,-0.024,-0.0129631448730622));
#30493=CARTESIAN_POINT('',(0.0210043631016192,-0.0327500380762009,-0.0137123694637889));
#30494=CARTESIAN_POINT('Origin',(0.01915000000001,-0.13898642901633,-0.0129631448730722));
#30495=CARTESIAN_POINT('Origin',(0.01915000000001,-0.0345723156209752,-0.0129631448730722));
#30496=CARTESIAN_POINT('Origin',(0.0211500000000181,-0.024,-0.00793218971944487));
#30497=CARTESIAN_POINT('',(0.0211500000000182,-0.02399999999999,-0.00800000000002138));
#30498=CARTESIAN_POINT('',(0.0211500000000147,-0.024,-0.00396609485971326));
#30499=CARTESIAN_POINT('',(0.0211500000000182,-0.0244065057553889,-0.00800000000000997));
#30500=CARTESIAN_POINT('',(0.0211500000000182,-0.024,-0.008));
#30501=CARTESIAN_POINT('',(0.0211500000000216,-0.0244065057541469,-0.0119660948595193));
#30502=CARTESIAN_POINT('Origin',(0.02715,-0.024,-0.00793218971944484));
#30503=CARTESIAN_POINT('',(0.0248178102805751,-0.03099999999999,-0.00793218971944484));
#30504=CARTESIAN_POINT('',(0.013575,-0.031,-0.00793218971944483));
#30505=CARTESIAN_POINT('',(0.0248178102805751,-0.03274999999999,-0.00793218971944484));
#30506=CARTESIAN_POINT('',(0.0248178102805552,-0.0284385814210553,-0.00793218971944484));
#30507=CARTESIAN_POINT('',(0.0247500000000101,-0.0328178102805551,-0.00793218971944484));
#30508=CARTESIAN_POINT('',(0.0275714051402776,-0.0299964051402776,-0.00793218971944484));
#30509=CARTESIAN_POINT('',(0.018825,-0.0328178102805552,-0.00793218971944484));
#30510=CARTESIAN_POINT('Origin',(0.016,-0.033,0.021));
#30511=CARTESIAN_POINT('',(0.00800000000000993,-0.0327500380762009,0.0210043631016193));
#30512=CARTESIAN_POINT('Origin',(-0.0155,-0.032875,0.0155));
#30513=CARTESIAN_POINT('',(-0.01850000000002,-0.03274999999999,0.01550000000001));
#30514=CARTESIAN_POINT('',(-0.0125000000000076,-0.0327499999999924,0.0155));
#30515=CARTESIAN_POINT('Origin',(-0.01550000000001,-0.03274999999999,0.01550000000001));
#30516=CARTESIAN_POINT('',(-0.0122499999999766,-0.0330000000000234,0.0155));
#30517=CARTESIAN_POINT('',(-0.012375,-0.032875,0.0155));
#30518=CARTESIAN_POINT('Origin',(-0.01550000000001,-0.033,0.01550000000001));
#30519=CARTESIAN_POINT('Origin',(-0.01550000000001,-0.033,0.01550000000001));
#30520=CARTESIAN_POINT('Origin',(-0.01550000000001,-0.03274999999999,0.01550000000001));
#30521=CARTESIAN_POINT('Origin',(-0.021,-0.033,0.016));
#30522=CARTESIAN_POINT('',(-0.0210043631016193,-0.0327500380762009,0.00800000000000997));
#30523=CARTESIAN_POINT('Origin',(-0.0208771815508047,-0.0328750190381054,
0.008));
#30524=CARTESIAN_POINT('',(-0.0207500000000101,-0.033,0.00800000000000997));
#30525=CARTESIAN_POINT('Origin',(-0.0155,-0.032875,-0.0155));
#30526=CARTESIAN_POINT('',(-0.01850000000002,-0.03274999999999,-0.0155000000000101));
#30527=CARTESIAN_POINT('',(-0.0125000000000076,-0.0327499999999924,-0.0155));
#30528=CARTESIAN_POINT('Origin',(-0.01550000000001,-0.03274999999999,-0.01550000000001));
#30529=CARTESIAN_POINT('',(-0.0122499999999766,-0.0330000000000234,-0.0155));
#30530=CARTESIAN_POINT('',(-0.012375,-0.032875,-0.0155));
#30531=CARTESIAN_POINT('Origin',(-0.01550000000001,-0.033,-0.01550000000001));
#30532=CARTESIAN_POINT('Origin',(-0.01550000000001,-0.033,-0.01550000000001));
#30533=CARTESIAN_POINT('Origin',(-0.01550000000001,-0.03274999999999,-0.01550000000001));
#30534=CARTESIAN_POINT('Origin',(-0.016,-0.033,-0.021));
#30535=CARTESIAN_POINT('',(-0.00800000000001002,-0.0327500380762009,-0.0210043631016193));
#30536=CARTESIAN_POINT('Origin',(-0.008,-0.0328750190381054,-0.0208771815508047));
#30537=CARTESIAN_POINT('',(-0.00800000000001002,-0.033,-0.02075000000001));
#30538=CARTESIAN_POINT('Origin',(0.0155,-0.032875,-0.0155));
#30539=CARTESIAN_POINT('',(0.0125,-0.03274999999999,-0.01550000000001));
#30540=CARTESIAN_POINT('',(0.0184999999999924,-0.0327499999999924,-0.0155));
#30541=CARTESIAN_POINT('Origin',(0.01550000000001,-0.03274999999999,-0.01550000000001));
#30542=CARTESIAN_POINT('',(0.0187500000000234,-0.0330000000000234,-0.0155));
#30543=CARTESIAN_POINT('',(0.018625,-0.032875,-0.0155));
#30544=CARTESIAN_POINT('Origin',(0.01550000000001,-0.033,-0.01550000000001));
#30545=CARTESIAN_POINT('Origin',(0.01550000000001,-0.033,-0.01550000000001));
#30546=CARTESIAN_POINT('Origin',(0.01550000000001,-0.03274999999999,-0.01550000000001));
#30547=CARTESIAN_POINT('Origin',(0.0208771815508047,-0.0328750190381054,
-0.008));
#30548=CARTESIAN_POINT('',(0.0210043631016093,-0.0327500380762109,-0.00799996192378907));
#30549=CARTESIAN_POINT('',(0.0210043631016192,-0.0327500380762009,-0.01200000000001));
#30550=CARTESIAN_POINT('',(0.02075,-0.033,-0.00775));
#30551=CARTESIAN_POINT('',(0.0191281314609001,-0.0345938057745268,-0.00615619422549322));
#30552=CARTESIAN_POINT('',(0.02075000000001,-0.033,-0.00800000000000997));
#30553=CARTESIAN_POINT('Origin',(0.021,-0.0327543256842211,-0.008));
#30554=CARTESIAN_POINT('',(0.021004363766232,-0.03275,-0.008));
#30555=CARTESIAN_POINT('',(0.01050000000001,-0.03274999999999,-0.00800000000000999));
#30556=CARTESIAN_POINT('',(0.0210349101298563,-0.031,-0.008));
#30557=CARTESIAN_POINT('',(0.0210006091729909,-0.0329651005032875,-0.00800000000000997));
#30558=CARTESIAN_POINT('',(0.0216250000000099,-0.03099999999999,-0.00800000000000997));
#30559=CARTESIAN_POINT('Origin',(0.0105,-0.032875,-0.007875));
#30560=CARTESIAN_POINT('',(0.02475,-0.033,-0.00775));
#30561=CARTESIAN_POINT('',(0.02475000000001,-0.03274999999999,-0.00800000000000996));
#30562=CARTESIAN_POINT('',(0.01050000000001,-0.033,-0.00775000000000998));
#30563=CARTESIAN_POINT('',(0.0210362867019386,-0.0309211362387957,-0.0098288637612043));
#30564=CARTESIAN_POINT('Origin',(0.024875,-0.033,0.007875));
#30565=CARTESIAN_POINT('',(0.025,-0.03275,0.00775));
#30566=CARTESIAN_POINT('',(0.02475000000001,-0.03274999999999,0.00800000000001004));
#30567=CARTESIAN_POINT('',(0.025,-0.031,0.00775));
#30568=CARTESIAN_POINT('',(0.02500000000001,-0.033,0.00775000000001004));
#30569=CARTESIAN_POINT('',(0.02062500000001,-0.03099999999999,0.01212500000001));
#30570=CARTESIAN_POINT('Origin',(-4.25999877636044E-17,-0.033,4.01748489384999E-31));
#30571=CARTESIAN_POINT('',(0.00800000000000993,-0.033,0.02075000000001));
#30572=CARTESIAN_POINT('',(0.02475,-0.033,0.00775));
#30573=CARTESIAN_POINT('',(0.02475000000001,-0.033,0.00400000000001004));
#30574=CARTESIAN_POINT('',(0.02075,-0.033,0.00775));
#30575=CARTESIAN_POINT('',(0.0105000000000099,-0.033,0.00775000000001002));
#30576=CARTESIAN_POINT('',(0.02075000000001,-0.033,-0.00800000000000997));
#30577=CARTESIAN_POINT('',(0.0187500000000234,-0.0330000000000234,0.0155));
#30578=CARTESIAN_POINT('Origin',(0.01550000000001,-0.033,0.01550000000001));
#30579=CARTESIAN_POINT('Origin',(0.01550000000001,-0.033,0.01550000000001));
#30580=CARTESIAN_POINT('',(-0.00450000000000004,-0.033,-7.38836374312403E-18));
#30581=CARTESIAN_POINT('Origin',(-4.48204338128547E-17,-0.033,3.98374757136611E-31));
#30582=CARTESIAN_POINT('Origin',(-0.0155,-0.03175,-0.0155));
#30583=CARTESIAN_POINT('',(-0.0185,-0.03049999999999,-0.0155));
#30584=CARTESIAN_POINT('Origin',(-0.01550000000001,-0.03049999999999,-0.01550000000001));
#30585=CARTESIAN_POINT('',(-0.0185,-0.03175,-0.0155));
#30586=CARTESIAN_POINT('Origin',(0.0155,-0.03175,-0.0155));
#30587=CARTESIAN_POINT('',(0.0125,-0.03049999999999,-0.0155));
#30588=CARTESIAN_POINT('Origin',(0.01550000000001,-0.03049999999999,-0.01550000000001));
#30589=CARTESIAN_POINT('',(0.0125,-0.03175,-0.0155));
#30590=CARTESIAN_POINT('Origin',(0.0155,-0.032875,0.0155));
#30591=CARTESIAN_POINT('',(0.0125,-0.03274999999999,0.01550000000001));
#30592=CARTESIAN_POINT('',(0.0184999999999924,-0.0327499999999924,0.0155));
#30593=CARTESIAN_POINT('Origin',(0.01550000000001,-0.03274999999999,0.01550000000001));
#30594=CARTESIAN_POINT('',(0.018625,-0.032875,0.0155));
#30595=CARTESIAN_POINT('Origin',(0.01550000000001,-0.03274999999999,0.01550000000001));
#30596=CARTESIAN_POINT('Origin',(0.0155,-0.03175,0.0155));
#30597=CARTESIAN_POINT('',(0.0125,-0.03049999999999,0.0155));
#30598=CARTESIAN_POINT('Origin',(0.01550000000001,-0.03049999999999,0.01550000000001));
#30599=CARTESIAN_POINT('',(0.0125,-0.03175,0.0155));
#30600=CARTESIAN_POINT('Origin',(-0.0155,-0.03175,0.0155));
#30601=CARTESIAN_POINT('',(-0.0185,-0.03049999999999,0.0155));
#30602=CARTESIAN_POINT('Origin',(-0.01550000000001,-0.03049999999999,0.01550000000001));
#30603=CARTESIAN_POINT('',(-0.0185,-0.03175,0.0155));
#30604=CARTESIAN_POINT('Origin',(0.0204055915910216,-0.024,0.01));
#30605=CARTESIAN_POINT('',(0.0189913780286485,-0.024,0.00858578643762694));
#30606=CARTESIAN_POINT('',(0.0204055915910216,-0.024,0.008));
#30607=CARTESIAN_POINT('Origin',(0.0204055915910316,-0.02399999999999,0.01000000000001));
#30608=CARTESIAN_POINT('',(0.0204055915910216,-0.031,0.008));
#30609=CARTESIAN_POINT('',(0.0204055915910316,-0.02399999999999,0.00800000000001003));
#30610=CARTESIAN_POINT('',(0.0189913780286485,-0.031,0.00858578643762694));
#30611=CARTESIAN_POINT('Origin',(0.0204055915910316,-0.03099999999999,0.01000000000001));
#30612=CARTESIAN_POINT('',(0.0189913780286585,-0.02399999999999,0.00858578643763693));
#30613=CARTESIAN_POINT('Origin',(0.025,-0.024,0.008));
#30614=CARTESIAN_POINT('',(0.0210349101298563,-0.031,0.008));
#30615=CARTESIAN_POINT('',(0.02100000000001,-0.033,0.00800000000001003));
#30616=CARTESIAN_POINT('',(0.02362500000001,-0.03099999999999,0.00800000000001004));
#30617=CARTESIAN_POINT('',(0.0125000000000099,-0.02399999999999,0.00800000000001002));
#30618=CARTESIAN_POINT('Origin',(-4.31418997390962E-17,-0.024,4.01513654477083E-31));
#30619=CARTESIAN_POINT('',(0.00807716446627529,-0.024,0.0195));
#30620=CARTESIAN_POINT('',(0.0166442911165788,-0.02399999999999,0.0109328733497165));
#30621=CARTESIAN_POINT('',(-0.00807716446627543,-0.024,0.0195));
#30622=CARTESIAN_POINT('',(0.0040385822331476,-0.02399999999999,0.01950000000001));
#30623=CARTESIAN_POINT('',(-0.0195,-0.024,0.00807716446627533));
#30624=CARTESIAN_POINT('',(-0.0109328733497166,-0.02399999999999,0.0166442911165788));
#30625=CARTESIAN_POINT('',(-0.0195,-0.024,-0.00807716446627539));
#30626=CARTESIAN_POINT('',(-0.0195000000000101,-0.02399999999999,0.00403858223314765));
#30627=CARTESIAN_POINT('',(-0.00807716446627538,-0.024,-0.0195));
#30628=CARTESIAN_POINT('',(-0.0166442911165788,-0.02399999999999,-0.0109328733497165));
#30629=CARTESIAN_POINT('',(0.00807716446627534,-0.024,-0.0195));
#30630=CARTESIAN_POINT('',(-0.00403858223314769,-0.02399999999999,-0.01950000000001));
#30631=CARTESIAN_POINT('',(0.0189913780286485,-0.024,-0.00858578643762688));
#30632=CARTESIAN_POINT('',(0.0109328733497165,-0.02399999999999,-0.0166442911165789));
#30633=CARTESIAN_POINT('',(0.0204055915910216,-0.024,-0.008));
#30634=CARTESIAN_POINT('Origin',(0.0204055915910316,-0.02399999999999,-0.01000000000001));
#30635=CARTESIAN_POINT('',(0.00975000000000998,-0.02399999999999,-0.00800000000000999));
#30636=CARTESIAN_POINT('',(0.0138,-0.02399999999999,-0.0155));
#30637=CARTESIAN_POINT('Origin',(0.01550000000001,-0.02399999999999,-0.01550000000001));
#30638=CARTESIAN_POINT('',(-0.0172,-0.02399999999999,0.0155));
#30639=CARTESIAN_POINT('Origin',(-0.01550000000001,-0.02399999999999,0.01550000000001));
#30640=CARTESIAN_POINT('',(0.0138,-0.02399999999999,0.0155));
#30641=CARTESIAN_POINT('Origin',(0.01550000000001,-0.02399999999999,0.01550000000001));
#30642=CARTESIAN_POINT('',(-0.0172,-0.02399999999999,-0.0155));
#30643=CARTESIAN_POINT('Origin',(-0.01550000000001,-0.02399999999999,-0.01550000000001));
#30644=CARTESIAN_POINT('Origin',(0.0204055915910216,-0.024,-0.01));
#30645=CARTESIAN_POINT('',(0.0189913780286485,-0.031,-0.00858578643762688));
#30646=CARTESIAN_POINT('',(0.0189913780286585,-0.02399999999999,-0.00858578643763687));
#30647=CARTESIAN_POINT('',(0.0204055915910216,-0.031,-0.008));
#30648=CARTESIAN_POINT('Origin',(0.0204055915910316,-0.03099999999999,-0.01000000000001));
#30649=CARTESIAN_POINT('',(0.0204055915910316,-0.02399999999999,-0.00800000000000997));
#30650=CARTESIAN_POINT('Origin',(0.00807716446627534,-0.024,-0.0195));
#30651=CARTESIAN_POINT('',(0.00807716446627534,-0.031,-0.0195));
#30652=CARTESIAN_POINT('',(0.00807716446628534,-0.02399999999999,-0.01950000000001));
#30653=CARTESIAN_POINT('',(0.0120208152801713,-0.031,-0.0155563491861041));
#30654=CARTESIAN_POINT('',(0.01950000000001,-0.03099999999999,-0.00807716446628533));
#30655=CARTESIAN_POINT('',(0.0120208152801713,-0.03,-0.0155563491861041));
#30656=CARTESIAN_POINT('',(0.0120208152801813,-0.03099999999999,-0.0155563491861141));
#30657=CARTESIAN_POINT('',(0.015556349186104,-0.03,-0.0120208152801713));
#30658=CARTESIAN_POINT('',(0.0109328733497165,-0.02999999999999,-0.0166442911165789));
#30659=CARTESIAN_POINT('',(0.015556349186104,-0.031,-0.0120208152801713));
#30660=CARTESIAN_POINT('',(0.0155563491861141,-0.03099999999999,-0.0120208152801813));
#30661=CARTESIAN_POINT('',(0.01950000000001,-0.03099999999999,-0.00807716446628533));
#30662=CARTESIAN_POINT('Origin',(0.0195,-0.024,-0.008));
#30663=CARTESIAN_POINT('',(0.02087500000001,-0.03099999999999,-0.00800000000000997));
#30664=CARTESIAN_POINT('',(0.0210006091729909,-0.0329651005032875,-0.00800000000000997));
#30665=CARTESIAN_POINT('Origin',(0.025,-0.03275,0.00775));
#30666=CARTESIAN_POINT('',(0.02475000000001,-0.033,0.00775000000001004));
#30667=CARTESIAN_POINT('',(0.02500000000001,-0.03274999999999,0.00775000000001004));
#30668=CARTESIAN_POINT('Origin',(0.02475,-0.03275,-0.008));
#30669=CARTESIAN_POINT('',(0.025,-0.03275,-0.00775));
#30670=CARTESIAN_POINT('',(0.02500000000001,-0.03274999999999,-0.00775000000000996));
#30671=CARTESIAN_POINT('',(0.02475000000001,-0.033,-0.00775000000000996));
#30672=CARTESIAN_POINT('Origin',(0.024875,-0.0328771628421105,-0.007875));
#30673=CARTESIAN_POINT('',(0.025,-0.031,-0.00775));
#30674=CARTESIAN_POINT('',(0.0206250000000099,-0.03099999999999,-0.01212500000001));
#30675=CARTESIAN_POINT('',(0.02500000000001,-0.0328771628421006,-0.00775000000000996));
#30676=CARTESIAN_POINT('Origin',(0.024875,-0.032875,0.004));
#30677=CARTESIAN_POINT('',(0.02500000000001,-0.03274999999999,0.00400000000001004));
#30678=CARTESIAN_POINT('Origin',(0.0105,-0.032875,0.007875));
#30679=CARTESIAN_POINT('',(0.021004363766232,-0.03275,0.008));
#30680=CARTESIAN_POINT('',(0.0105000000000099,-0.03274999999999,0.00800000000001002));
#30681=CARTESIAN_POINT('',(0.0210043631016093,-0.0327500380762109,0.00799996192378913));
#30682=CARTESIAN_POINT('',(0.0208966674520598,-0.0389199177072798,0.00183008229274029));
#30683=CARTESIAN_POINT('',(0.01644626929095,-0.0372292643889901,0.00352073561102997));
#30684=CARTESIAN_POINT('Origin',(0.0175,-0.031,-0.0065));
#30685=CARTESIAN_POINT('',(0.0175,-0.0328,-0.007));
#30686=CARTESIAN_POINT('',(0.017,-0.0328,-0.0065));
#30687=CARTESIAN_POINT('Origin',(0.01750000000001,-0.03279999999999,-0.00650000000000997));
#30688=CARTESIAN_POINT('',(0.0175,-0.031,-0.007));
#30689=CARTESIAN_POINT('',(0.01750000000001,-0.03099999999999,-0.00700000000000997));
#30690=CARTESIAN_POINT('',(0.017,-0.031,-0.0065));
#30691=CARTESIAN_POINT('Origin',(0.01750000000001,-0.03099999999999,-0.00650000000000997));
#30692=CARTESIAN_POINT('',(0.01700000000001,-0.03099999999999,-0.00650000000000997));
#30693=CARTESIAN_POINT('Origin',(0.017,-0.031,-0.007));
#30694=CARTESIAN_POINT('',(0.0235,-0.0328,-0.007));
#30695=CARTESIAN_POINT('',(0.02400000000001,-0.03279999999999,-0.00700000000000996));
#30696=CARTESIAN_POINT('',(0.0235,-0.031,-0.007));
#30697=CARTESIAN_POINT('',(0.02350000000001,-0.03099999999999,-0.00700000000000996));
#30698=CARTESIAN_POINT('',(0.00850000000000998,-0.03099999999999,-0.00700000000000999));
#30699=CARTESIAN_POINT('Origin',(0.0235,-0.031,-0.0065));
#30700=CARTESIAN_POINT('',(0.024,-0.0328,-0.0065));
#30701=CARTESIAN_POINT('Origin',(0.02350000000001,-0.03279999999999,-0.00650000000000996));
#30702=CARTESIAN_POINT('',(0.024,-0.031,-0.0065));
#30703=CARTESIAN_POINT('',(0.02400000000001,-0.03099999999999,-0.00650000000000996));
#30704=CARTESIAN_POINT('Origin',(0.02350000000001,-0.03099999999999,-0.00650000000000996));
#30705=CARTESIAN_POINT('Origin',(0.024,-0.031,-0.007));
#30706=CARTESIAN_POINT('',(0.024,-0.0328,0.0065));
#30707=CARTESIAN_POINT('',(0.02400000000001,-0.03279999999999,0.00700000000001004));
#30708=CARTESIAN_POINT('',(0.024,-0.031,0.0065));
#30709=CARTESIAN_POINT('',(0.02400000000001,-0.03099999999999,0.00650000000001004));
#30710=CARTESIAN_POINT('',(0.02400000000001,-0.03099999999999,-0.00350000000000997));
#30711=CARTESIAN_POINT('Origin',(0.0235,-0.031,0.0065));
#30712=CARTESIAN_POINT('',(0.0235,-0.0328,0.007));
#30713=CARTESIAN_POINT('Origin',(0.02350000000001,-0.03279999999999,0.00650000000001004));
#30714=CARTESIAN_POINT('',(0.0235,-0.031,0.007));
#30715=CARTESIAN_POINT('',(0.02350000000001,-0.03099999999999,0.00700000000001004));
#30716=CARTESIAN_POINT('Origin',(0.02350000000001,-0.03099999999999,0.00650000000001004));
#30717=CARTESIAN_POINT('Origin',(0.024,-0.031,0.007));
#30718=CARTESIAN_POINT('',(0.0175,-0.0328,0.007));
#30719=CARTESIAN_POINT('',(0.01700000000001,-0.03279999999999,0.00700000000001003));
#30720=CARTESIAN_POINT('',(0.0175,-0.031,0.007));
#30721=CARTESIAN_POINT('',(0.01750000000001,-0.03099999999999,0.00700000000001003));
#30722=CARTESIAN_POINT('',(0.0120000000000099,-0.03099999999999,0.00700000000001002));
#30723=CARTESIAN_POINT('Origin',(0.0175,-0.031,0.0065));
#30724=CARTESIAN_POINT('',(0.017,-0.0328,0.0065));
#30725=CARTESIAN_POINT('Origin',(0.01750000000001,-0.03279999999999,0.00650000000001003));
#30726=CARTESIAN_POINT('',(0.017,-0.031,0.0065));
#30727=CARTESIAN_POINT('',(0.01700000000001,-0.03099999999999,0.00650000000001003));
#30728=CARTESIAN_POINT('Origin',(0.01750000000001,-0.03099999999999,0.00650000000001003));
#30729=CARTESIAN_POINT('Origin',(0.0205,-0.0328,3.1147575558204E-17));
#30730=CARTESIAN_POINT('',(0.01700000000001,-0.03279999999999,-0.00700000000000997));
#30731=CARTESIAN_POINT('Origin',(0.017,-0.031,0.007));
#30732=CARTESIAN_POINT('',(0.01700000000001,-0.03099999999999,0.00350000000001003));
#30733=CARTESIAN_POINT('Origin',(0.021,-0.033,-0.016));
#30734=CARTESIAN_POINT('Origin',(0.0208771815508047,-0.0328750190381054,
-0.008));
#30735=CARTESIAN_POINT('',(0.0210043631016192,-0.0327500380762009,-0.00800000000000997));
#30736=CARTESIAN_POINT('Origin',(-4.84735884755548E-17,0.0276710931871507,
3.96791680405306E-31));
#30737=CARTESIAN_POINT('',(-0.00450000000000004,-0.03199999999999,-7.38836374312403E-18));
#30738=CARTESIAN_POINT('Origin',(-4.48806462545766E-17,-0.03199999999999,
3.98348664369065E-31));
#30739=CARTESIAN_POINT('',(-0.00450000000000005,0.0276710931871507,-7.38836374312403E-18));
#30740=CARTESIAN_POINT('Origin',(0.021,-0.033,0.008));
#30741=CARTESIAN_POINT('',(0.0216250000000099,-0.03099999999999,0.00800000000001003));
#30742=CARTESIAN_POINT('',(0.02100000000001,-0.033,0.00800000000001003));
#30743=CARTESIAN_POINT('Origin',(0.025,-0.033,0.008));
#30744=CARTESIAN_POINT('',(0.02500000000001,-0.03099999999999,0.00400000000001004));
#30745=CARTESIAN_POINT('Origin',(0.0155,-0.031,0.0155));
#30746=CARTESIAN_POINT('',(0.0120208152801712,-0.031,0.0155563491861041));
#30747=CARTESIAN_POINT('',(0.015556349186104,-0.031,0.0120208152801713));
#30748=CARTESIAN_POINT('Origin',(0.01550000000001,-0.03099999999999,0.01550000000001));
#30749=CARTESIAN_POINT('',(0.0120208152801712,-0.03,0.0155563491861041));
#30750=CARTESIAN_POINT('',(0.0120208152801812,-0.03099999999999,0.0155563491861141));
#30751=CARTESIAN_POINT('',(0.015556349186104,-0.03,0.0120208152801713));
#30752=CARTESIAN_POINT('Origin',(0.01550000000001,-0.02999999999999,0.01550000000001));
#30753=CARTESIAN_POINT('',(0.0155563491861141,-0.03099999999999,0.0120208152801813));
#30754=CARTESIAN_POINT('Origin',(0.0137883540889866,-0.03,0.0137883540889867));
#30755=CARTESIAN_POINT('',(0.0166442911165788,-0.02999999999999,0.0109328733497165));
#30756=CARTESIAN_POINT('Origin',(0.0155,-0.031,-0.0155));
#30757=CARTESIAN_POINT('Origin',(0.01550000000001,-0.03099999999999,-0.01550000000001));
#30758=CARTESIAN_POINT('Origin',(0.01550000000001,-0.02999999999999,-0.01550000000001));
#30759=CARTESIAN_POINT('Origin',(0.0137883540889867,-0.03,-0.0137883540889867));
#30760=CARTESIAN_POINT('Origin',(-0.0155,-0.031,-0.0155));
#30761=CARTESIAN_POINT('',(-0.0120208152801713,-0.031,-0.0155563491861041));
#30762=CARTESIAN_POINT('',(-0.0155563491861042,-0.031,-0.0120208152801713));
#30763=CARTESIAN_POINT('Origin',(-0.01550000000001,-0.03099999999999,-0.01550000000001));
#30764=CARTESIAN_POINT('',(-0.0120208152801713,-0.03,-0.0155563491861041));
#30765=CARTESIAN_POINT('',(-0.0120208152801813,-0.03099999999999,-0.0155563491861141));
#30766=CARTESIAN_POINT('',(-0.0155563491861042,-0.03,-0.0120208152801713));
#30767=CARTESIAN_POINT('Origin',(-0.01550000000001,-0.02999999999999,-0.01550000000001));
#30768=CARTESIAN_POINT('',(-0.0155563491861142,-0.03099999999999,-0.0120208152801813));
#30769=CARTESIAN_POINT('Origin',(-0.0137883540889867,-0.03,-0.0137883540889867));
#30770=CARTESIAN_POINT('',(-0.0166442911165788,-0.02999999999999,-0.0109328733497165));
#30771=CARTESIAN_POINT('Origin',(0.0195,-0.024,0.00807716446627539));
#30772=CARTESIAN_POINT('',(0.00807716446628528,-0.03099999999999,0.01950000000001));
#30773=CARTESIAN_POINT('',(0.00807716446627529,-0.031,0.0195));
#30774=CARTESIAN_POINT('',(0.00807716446628528,-0.03099999999999,0.01950000000001));
#30775=CARTESIAN_POINT('',(0.00807716446628528,-0.02399999999999,0.01950000000001));
#30776=CARTESIAN_POINT('Origin',(-0.0195,-0.024,-0.00807716446627539));
#30777=CARTESIAN_POINT('',(-0.00807716446627538,-0.031,-0.0195));
#30778=CARTESIAN_POINT('',(-0.00807716446628537,-0.03099999999999,-0.01950000000001));
#30779=CARTESIAN_POINT('',(-0.00807716446628537,-0.02399999999999,-0.01950000000001));
#30780=CARTESIAN_POINT('',(-0.0195,-0.031,-0.00807716446627539));
#30781=CARTESIAN_POINT('',(-0.0195000000000101,-0.02399999999999,-0.00807716446628539));
#30782=CARTESIAN_POINT('',(-0.00807716446628537,-0.03099999999999,-0.01950000000001));
#30783=CARTESIAN_POINT('Origin',(-0.0155,-0.031,0.0155));
#30784=CARTESIAN_POINT('',(-0.0155563491861042,-0.031,0.0120208152801713));
#30785=CARTESIAN_POINT('',(-0.0120208152801714,-0.031,0.0155563491861041));
#30786=CARTESIAN_POINT('Origin',(-0.01550000000001,-0.03099999999999,0.01550000000001));
#30787=CARTESIAN_POINT('',(-0.0155563491861042,-0.03,0.0120208152801713));
#30788=CARTESIAN_POINT('',(-0.0155563491861142,-0.03099999999999,0.0120208152801813));
#30789=CARTESIAN_POINT('',(-0.0120208152801714,-0.03,0.0155563491861041));
#30790=CARTESIAN_POINT('Origin',(-0.01550000000001,-0.02999999999999,0.01550000000001));
#30791=CARTESIAN_POINT('',(-0.0120208152801814,-0.03099999999999,0.0155563491861141));
#30792=CARTESIAN_POINT('Origin',(-0.0137883540889868,-0.03,0.0137883540889867));
#30793=CARTESIAN_POINT('',(-0.0109328733497166,-0.02999999999999,0.0166442911165789));
#30794=CARTESIAN_POINT('Origin',(-0.00807716446627543,-0.024,0.0195));
#30795=CARTESIAN_POINT('',(-0.0195,-0.031,0.00807716446627533));
#30796=CARTESIAN_POINT('',(-0.0195000000000101,-0.03099999999999,0.00807716446628533));
#30797=CARTESIAN_POINT('',(-0.0195000000000101,-0.02399999999999,0.00807716446628533));
#30798=CARTESIAN_POINT('',(-0.00807716446627543,-0.031,0.0195));
#30799=CARTESIAN_POINT('',(-0.00807716446628543,-0.02399999999999,0.01950000000001));
#30800=CARTESIAN_POINT('',(-0.0195000000000101,-0.03099999999999,0.00807716446628533));
#30801=CARTESIAN_POINT('Origin',(0.008,-0.0328750190381054,0.0208771815508047));
#30802=CARTESIAN_POINT('Origin',(-4.54150316748527E-17,-0.023125,3.98117091057093E-31));
#30803=CARTESIAN_POINT('',(0.013,-0.02325,2.13441619245821E-17));
#30804=CARTESIAN_POINT('Origin',(-4.54075051196382E-17,-0.02324999999999,
3.98120352653036E-31));
#30805=CARTESIAN_POINT('',(0.01275,-0.023,2.09336972721863E-17));
#30806=CARTESIAN_POINT('',(0.012875,-0.023125,2.11389295983842E-17));
#30807=CARTESIAN_POINT('Origin',(-4.54225582300685E-17,-0.02299999999999,
3.98113829461149E-31));
#30808=CARTESIAN_POINT('Origin',(-4.54225582300679E-17,-0.023,3.9811382946115E-31));
#30809=CARTESIAN_POINT('',(0.0082500000000029,-0.0229999999999882,1.15246663104728E-17));
#30810=CARTESIAN_POINT('Origin',(-4.54225582300685E-17,-0.02299999999999,
3.98113829461149E-31));
#30811=CARTESIAN_POINT('Origin',(-4.53623457883466E-17,-0.024,3.98139922228696E-31));
#30812=CARTESIAN_POINT('',(0.013,-0.03099999999999,2.13441619245821E-17));
#30813=CARTESIAN_POINT('Origin',(-4.49408586962979E-17,-0.03099999999999,
3.98322571601518E-31));
#30814=CARTESIAN_POINT('',(0.013,-0.024,2.13441619245821E-17));
#30815=CARTESIAN_POINT('Origin',(-4.53924520092072E-17,-0.0235,3.98126875844923E-31));
#30816=CARTESIAN_POINT('',(-0.00800000000001005,-0.02399999999999,-1.21551514373626E-17));
#30817=CARTESIAN_POINT('',(0.0080000000000029,-0.0239999999999882,1.11754339980344E-17));
#30818=CARTESIAN_POINT('Origin',(-4.53623457883472E-17,-0.02399999999999,
3.98139922228695E-31));
#30819=CARTESIAN_POINT('',(0.00812499999999996,-0.0235,1.13500501542495E-17));
#30820=CARTESIAN_POINT('Origin',(-4.53623457883472E-17,-0.02399999999999,
3.98139922228695E-31));
#30821=CARTESIAN_POINT('Origin',(-4.54225582300679E-17,-0.023,3.9811382946115E-31));
#30822=CARTESIAN_POINT('',(-0.00800000000000005,-0.03124999999999,-1.31348688766652E-17));
#30823=CARTESIAN_POINT('',(-0.00800000000000005,-0.023,-1.31348688766652E-17));
#30824=CARTESIAN_POINT('Origin',(-4.49258055858676E-17,-0.03124999999999,
3.98329094793405E-31));
#30825=CARTESIAN_POINT('Origin',(0.0155,-0.0305,-0.0155));
#30826=CARTESIAN_POINT('',(0.0138,-0.03049999999999,-0.0155));
#30827=CARTESIAN_POINT('Origin',(0.01550000000001,-0.03049999999999,-0.01550000000001));
#30828=CARTESIAN_POINT('Origin',(0.0155,0.0276710931871507,-0.0155));
#30829=CARTESIAN_POINT('',(0.0138,0.0276710931871507,-0.0155));
#30830=CARTESIAN_POINT('Origin',(-0.0155,-0.0305,0.0155));
#30831=CARTESIAN_POINT('',(-0.0172,-0.03049999999999,0.0155));
#30832=CARTESIAN_POINT('Origin',(-0.01550000000001,-0.03049999999999,0.01550000000001));
#30833=CARTESIAN_POINT('Origin',(-0.0155,0.0276710931871507,0.0155));
#30834=CARTESIAN_POINT('',(-0.0172,0.0276710931871507,0.0155));
#30835=CARTESIAN_POINT('Origin',(0.0155,-0.0305,0.0155));
#30836=CARTESIAN_POINT('',(0.0138,-0.03049999999999,0.0155));
#30837=CARTESIAN_POINT('Origin',(0.01550000000001,-0.03049999999999,0.01550000000001));
#30838=CARTESIAN_POINT('Origin',(0.0155,0.0276710931871507,0.0155));
#30839=CARTESIAN_POINT('',(0.0138,0.0276710931871507,0.0155));
#30840=CARTESIAN_POINT('Origin',(-0.0155,-0.0305,-0.0155));
#30841=CARTESIAN_POINT('',(-0.0172,-0.03049999999999,-0.0155));
#30842=CARTESIAN_POINT('Origin',(-0.01550000000001,-0.03049999999999,-0.01550000000001));
#30843=CARTESIAN_POINT('Origin',(-0.0155,0.0276710931871507,-0.0155));
#30844=CARTESIAN_POINT('',(-0.0172,0.0276710931871507,-0.0155));
#30845=CARTESIAN_POINT('Origin',(-4.16101896224218E-17,-0.031,1.11022302462556E-18));
#30846=CARTESIAN_POINT('',(0.00807716446628534,-0.03099999999999,-0.01950000000001));
#30847=CARTESIAN_POINT('',(-0.0195000000000101,-0.03099999999999,-0.00807716446628539));
#30848=CARTESIAN_POINT('',(-0.00807716446628543,-0.03099999999999,0.01950000000001));
#30849=CARTESIAN_POINT('Origin',(-4.4925805585867E-17,-0.03125,3.98329094793406E-31));
#30850=CARTESIAN_POINT('',(-0.00600000000000004,-0.03124999999999,-9.85115165749883E-18));
#30851=CARTESIAN_POINT('Origin',(-4.49258055858676E-17,-0.03124999999999,
3.98329094793405E-31));
#30852=CARTESIAN_POINT('',(-0.00600000000000004,-0.03199999999999,-9.85115165749883E-18));
#30853=CARTESIAN_POINT('',(-0.00600000000000004,-0.03125,-9.85115165749883E-18));
#30854=CARTESIAN_POINT('Origin',(-4.48806462545766E-17,-0.03199999999999,
3.98348664369065E-31));
#30855=CARTESIAN_POINT('Origin',(-4.4880646254576E-17,-0.032,3.98348664369065E-31));
#30856=CARTESIAN_POINT('Origin',(-4.4925805585867E-17,-0.03125,3.98329094793406E-31));
#30857=CARTESIAN_POINT('Origin',(-0.00807716446627538,-0.024,-0.0195));
#30858=CARTESIAN_POINT('Origin',(-0.0195,-0.024,0.00807716446627533));
#30859=CARTESIAN_POINT('Origin',(0.00807716446627529,-0.024,0.0195));
#30860=CARTESIAN_POINT('Origin',(0.021,-0.033,-0.016));
#30861=CARTESIAN_POINT('',(0.,0.,0.));
#30862=CARTESIAN_POINT('Origin',(-4.34919666873154E-17,-0.030975,7.19534755436855E-33));
#30863=CARTESIAN_POINT('',(-1.20316693238282E-7,-0.03125000000001,0.00772499999907304));
#30864=CARTESIAN_POINT('Origin',(-4.34751277937011E-17,-0.03125000000001,
7.20399477813186E-33));
#30865=CARTESIAN_POINT('',(-1.24599811766264E-7,-0.03097500000001,0.00799999999903968));
#30866=CARTESIAN_POINT('Origin',(-1.20316693238144E-7,-0.030975,0.00772499999906304));
#30867=CARTESIAN_POINT('',(-0.00799999999903972,-0.03097500000001,-1.24599801720813E-7));
#30868=CARTESIAN_POINT('Origin',(-4.34919666873148E-17,-0.03097500000001,
7.19534755436887E-33));
#30869=CARTESIAN_POINT('Origin',(-4.34919666873148E-17,-0.03097500000001,
7.19534755436887E-33));
#30870=CARTESIAN_POINT('Origin',(-4.36282086447352E-17,-0.02875,7.12538365301343E-33));
#30871=CARTESIAN_POINT('',(-0.00799999999903972,-0.02652500000001,-1.24599801720813E-7));
#30872=CARTESIAN_POINT('',(-0.00799999999902972,-0.02875,-1.24599811722617E-7));
#30873=CARTESIAN_POINT('',(-1.24599811766537E-7,-0.02652500000001,0.00799999999903968));
#30874=CARTESIAN_POINT('Origin',(-4.37644506021545E-17,-0.02652500000001,
7.05541975165862E-33));
#30875=CARTESIAN_POINT('Origin',(-4.37644506021545E-17,-0.02652500000001,
7.05541975165862E-33));
#30876=CARTESIAN_POINT('Origin',(0.00708333333247415,-0.03125,1.10322749961866E-7));
#30877=CARTESIAN_POINT('',(-0.00616666666591875,-0.03125000000001,-9.60456882028501E-8));
#30878=CARTESIAN_POINT('Origin',(-4.34751277937011E-17,-0.03125000000001,
7.20399477813186E-33));
#30879=CARTESIAN_POINT('Origin',(-4.37644506021551E-17,-0.026525,7.0554197516583E-33));
#30880=CARTESIAN_POINT('',(-1.20316693238589E-7,-0.02625000000001,0.00772499999907304));
#30881=CARTESIAN_POINT('Origin',(-1.20316693238416E-7,-0.026525,0.00772499999906304));
#30882=CARTESIAN_POINT('Origin',(-4.37812894957682E-17,-0.02625000000001,
7.04677252789562E-33));
#30883=CARTESIAN_POINT('Origin',(0.00708333333247415,-0.02625,1.10322749961866E-7));
#30884=CARTESIAN_POINT('',(-0.00616666666591875,-0.02625000000001,-9.60456882028501E-8));
#30885=CARTESIAN_POINT('Origin',(-4.37812894957682E-17,-0.02625000000001,
7.04677252789562E-33));
#30886=CARTESIAN_POINT('Origin',(-4.36282086447352E-17,-0.02875,7.12538365301343E-33));
#30887=CARTESIAN_POINT('',(-0.00616666666591875,-0.02875,-9.60456882028501E-8));
#30888=CARTESIAN_POINT('',(0.,0.,0.));
#30889=CARTESIAN_POINT('Origin',(0.02115,-0.0223,-0.01175));
#30890=CARTESIAN_POINT('',(0.02115,-0.02545,0.00474999999999993));
#30891=CARTESIAN_POINT('',(0.02115,-0.02545,0.00524999999999993));
#30892=CARTESIAN_POINT('',(0.02115000000001,-0.02545000000001,-0.00349999999999003));
#30893=CARTESIAN_POINT('',(0.02115,-0.0317,0.00524999999999993));
#30894=CARTESIAN_POINT('',(0.0211500000000101,-0.02422500000001,0.00525000000000993));
#30895=CARTESIAN_POINT('',(0.02115,-0.0317,0.00474999999999993));
#30896=CARTESIAN_POINT('',(0.0211500000000101,-0.0317000000000099,-0.00549999999999003));
#30897=CARTESIAN_POINT('',(0.0211500000000101,-0.02545000000001,0.00475000000000993));
#30898=CARTESIAN_POINT('Origin',(0.02115,-0.0317,0.000749999999999928));
#30899=CARTESIAN_POINT('',(0.02065,-0.0317,0.00524999999999993));
#30900=CARTESIAN_POINT('',(0.0206500000000101,-0.03170000000001,0.00525000000000993));
#30901=CARTESIAN_POINT('',(0.02065,-0.0317,0.00474999999999993));
#30902=CARTESIAN_POINT('',(0.0206500000000101,-0.03170000000001,0.00525000000000993));
#30903=CARTESIAN_POINT('',(0.0206500000000101,-0.03170000000001,0.00475000000000993));
#30904=CARTESIAN_POINT('Origin',(0.02115,-0.02545,0.00499999999999993));
#30905=CARTESIAN_POINT('',(0.02115,-0.02495,0.00474999999999993));
#30906=CARTESIAN_POINT('',(0.02115,-0.02495,0.00524999999999993));
#30907=CARTESIAN_POINT('',(0.02115000000001,-0.02495000000001,0.00525000000000993));
#30908=CARTESIAN_POINT('',(0.02065,-0.02545,0.00474999999999993));
#30909=CARTESIAN_POINT('Origin',(0.0211500000000101,-0.02545000000001,0.00475000000000993));
#30910=CARTESIAN_POINT('',(0.02065,-0.02545,0.00524999999999993));
#30911=CARTESIAN_POINT('',(0.0206500000000101,-0.02545000000001,0.00525000000000993));
#30912=CARTESIAN_POINT('Origin',(0.02115000000001,-0.02545000000001,0.00525000000000993));
#30913=CARTESIAN_POINT('Origin',(0.02065,-0.02545,0.00524999999999993));
#30914=CARTESIAN_POINT('',(0.0206500000000101,-0.02545000000001,0.00475000000000993));
#30915=CARTESIAN_POINT('',(0.0206500000000101,-0.02545000000001,0.00525000000000993));
#30916=CARTESIAN_POINT('Origin',(0.0229,-0.02545,0.00474999999999991));
#30917=CARTESIAN_POINT('',(0.0262,-0.02495,0.00474999999999988));
#30918=CARTESIAN_POINT('',(0.0229000000000101,-0.02495000000001,0.00475000000000991));
#30919=CARTESIAN_POINT('',(0.0262,-0.02545,0.00474999999999988));
#30920=CARTESIAN_POINT('',(0.0262000000000101,-0.02495000000001,0.00475000000000998));
#30921=CARTESIAN_POINT('',(0.0229000000000101,-0.02545000000001,0.00475000000000991));
#30922=CARTESIAN_POINT('Origin',(0.0229,-0.02545,0.00524999999999991));
#30923=CARTESIAN_POINT('',(0.0262,-0.02545,0.00524999999999988));
#30924=CARTESIAN_POINT('',(0.0262000000000101,-0.02545000000001,0.00475000000000998));
#30925=CARTESIAN_POINT('',(0.0229000000000101,-0.02545000000001,0.00525000000000991));
#30926=CARTESIAN_POINT('Origin',(0.0229,-0.02495,0.00524999999999991));
#30927=CARTESIAN_POINT('',(0.0262,-0.02495,0.00524999999999988));
#30928=CARTESIAN_POINT('',(0.0262000000000101,-0.02545000000001,0.00525000000000998));
#30929=CARTESIAN_POINT('',(0.0229000000000101,-0.02495000000001,0.00525000000000991));
#30930=CARTESIAN_POINT('Origin',(0.0229,-0.02495,0.00474999999999991));
#30931=CARTESIAN_POINT('',(0.0262000000000101,-0.02495000000001,0.00525000000000998));
#30932=CARTESIAN_POINT('Origin',(0.0262,-0.0252,0.00499999999999988));
#30933=CARTESIAN_POINT('',(0.,0.,0.));
#30934=CARTESIAN_POINT('Origin',(0.02065,-0.02545,0.00324999999999993));
#30935=CARTESIAN_POINT('',(0.02065,-0.02545,0.00274999999999993));
#30936=CARTESIAN_POINT('',(0.02065,-0.02545,0.00324999999999993));
#30937=CARTESIAN_POINT('',(0.0206500000000101,-0.02545000000001,0.00325000000000994));
#30938=CARTESIAN_POINT('',(0.02065,-0.0317,0.00274999999999993));
#30939=CARTESIAN_POINT('',(0.0206500000000101,-0.02545000000001,0.00275000000000994));
#30940=CARTESIAN_POINT('',(0.02065,-0.0317,0.00324999999999993));
#30941=CARTESIAN_POINT('',(0.0206500000000101,-0.03170000000001,0.00325000000000994));
#30942=CARTESIAN_POINT('',(0.0206500000000101,-0.02545000000001,0.00325000000000994));
#30943=CARTESIAN_POINT('Origin',(0.02115,-0.02495,0.00324999999999992));
#30944=CARTESIAN_POINT('',(0.02115,-0.02495,0.00324999999999992));
#30945=CARTESIAN_POINT('Origin',(0.02115000000001,-0.02545000000001,0.00325000000000992));
#30946=CARTESIAN_POINT('',(0.02115,-0.0317,0.00324999999999992));
#30947=CARTESIAN_POINT('',(0.0206500000000101,-0.03170000000001,0.00325000000000994));
#30948=CARTESIAN_POINT('',(0.02115,-0.02545,0.00324999999999992));
#30949=CARTESIAN_POINT('',(0.02115000000001,-0.02545000000001,0.00325000000000992));
#30950=CARTESIAN_POINT('',(0.0262,-0.02545,0.00324999999999987));
#30951=CARTESIAN_POINT('',(0.0229000000000101,-0.02545000000001,0.00325000000000991));
#30952=CARTESIAN_POINT('',(0.0262,-0.02495,0.00324999999999987));
#30953=CARTESIAN_POINT('',(0.0262000000000101,-0.02545000000001,0.00325000000000997));
#30954=CARTESIAN_POINT('',(0.0229000000000101,-0.02495000000001,0.00325000000000991));
#30955=CARTESIAN_POINT('Origin',(0.02115,-0.02545,0.00299999999999993));
#30956=CARTESIAN_POINT('',(0.02115,-0.02495,0.00274999999999993));
#30957=CARTESIAN_POINT('',(0.0211500000000101,-0.02495000000001,0.00325000000000992));
#30958=CARTESIAN_POINT('Origin',(0.0211500000000101,-0.02545000000001,0.00275000000000993));
#30959=CARTESIAN_POINT('Origin',(0.02115,-0.02495,0.00274999999999993));
#30960=CARTESIAN_POINT('',(0.02115,-0.02545,0.00274999999999993));
#30961=CARTESIAN_POINT('',(0.02115,-0.0317,0.00274999999999993));
#30962=CARTESIAN_POINT('',(0.0211500000000101,-0.02545000000001,0.00275000000000993));
#30963=CARTESIAN_POINT('',(0.0206500000000101,-0.03170000000001,0.00275000000000994));
#30964=CARTESIAN_POINT('',(0.0262,-0.02495,0.00274999999999987));
#30965=CARTESIAN_POINT('',(0.0229000000000101,-0.02495000000001,0.00275000000000991));
#30966=CARTESIAN_POINT('',(0.0262,-0.02545,0.00274999999999987));
#30967=CARTESIAN_POINT('',(0.0262000000000101,-0.02495000000001,0.00275000000000997));
#30968=CARTESIAN_POINT('',(0.0229000000000101,-0.02545000000001,0.00275000000000991));
#30969=CARTESIAN_POINT('Origin',(0.02115,-0.0317,0.000749999999999928));
#30970=CARTESIAN_POINT('',(0.0211500000000101,-0.0317000000000099,-0.00549999999999003));
#30971=CARTESIAN_POINT('Origin',(0.02115,-0.0223,-0.01175));
#30972=CARTESIAN_POINT('',(0.0211500000000101,-0.02545000000001,-0.00449999999999003));
#30973=CARTESIAN_POINT('Origin',(0.0229,-0.02545,0.00324999999999991));
#30974=CARTESIAN_POINT('',(0.0262000000000101,-0.02545000000001,0.00275000000000997));
#30975=CARTESIAN_POINT('Origin',(0.0229,-0.02495,0.00274999999999991));
#30976=CARTESIAN_POINT('',(0.0262000000000101,-0.02495000000001,0.00325000000000997));
#30977=CARTESIAN_POINT('Origin',(0.0262,-0.0252,0.00299999999999988));
#30978=CARTESIAN_POINT('',(0.,0.,0.));
#30979=CARTESIAN_POINT('Origin',(-4.35815392021282E-17,-0.02565,3.46944695195361E-18));
#30980=CARTESIAN_POINT('',(-0.00339852988617145,-0.02625,-0.00255195897553229));
#30981=CARTESIAN_POINT('',(0.00337017181023001,-0.02625,-0.00258929372021227));
#30982=CARTESIAN_POINT('Origin',(9.90123578286685E-15,-0.02625000000001,
-1.00514215006786E-14));
#30983=CARTESIAN_POINT('',(0.00337017181023001,-0.02565,-0.00258929372021227));
#30984=CARTESIAN_POINT('',(0.00337017181023996,-0.02565,-0.00258929372022232));
#30985=CARTESIAN_POINT('',(-0.00339852988617145,-0.02565,-0.00255195897553229));
#30986=CARTESIAN_POINT('Origin',(9.90111042199066E-15,-0.02565,-1.00514215006786E-14));
#30987=CARTESIAN_POINT('',(-0.0033985298861815,-0.02565,-0.00255195897554223));
#30988=CARTESIAN_POINT('Origin',(0.00290627757282187,-0.02565,-0.00223288505519481));
#30989=CARTESIAN_POINT('',(0.00235396717919693,-0.02625,-0.00242570162370972));
#30990=CARTESIAN_POINT('Origin',(0.00290627757283182,-0.02625000000001,
-0.00223288505520486));
#30991=CARTESIAN_POINT('',(0.00235396717919693,-0.02565,-0.00242570162370972));
#30992=CARTESIAN_POINT('',(0.00235396717920687,-0.02565,-0.00242570162371977));
#30993=CARTESIAN_POINT('Origin',(0.00290627757283182,-0.02565,-0.00223288505520486));
#30994=CARTESIAN_POINT('Origin',(0.00235396717919693,-0.02565,-0.00242570162370972));
#30995=CARTESIAN_POINT('',(0.00178287508311634,-0.02625,-0.000789845831794254));
#30996=CARTESIAN_POINT('',(0.00178287508312629,-0.02625000000001,-0.000789845831804309));
#30997=CARTESIAN_POINT('',(0.00178287508311634,-0.02565,-0.000789845831794254));
#30998=CARTESIAN_POINT('',(0.00178287508312629,-0.02565,-0.000789845831804309));
#30999=CARTESIAN_POINT('',(0.00178287508312629,-0.02565,-0.000789845831804309));
#31000=CARTESIAN_POINT('Origin',(-4.35815392021282E-17,-0.02565,3.46944695195361E-18));
#31001=CARTESIAN_POINT('',(0.00185038829705699,-0.02625,0.000615274857372195));
#31002=CARTESIAN_POINT('Origin',(9.90123578286685E-15,-0.02625000000001,
-1.00514215006786E-14));
#31003=CARTESIAN_POINT('',(0.00185038829705699,-0.02565,0.000615274857372195));
#31004=CARTESIAN_POINT('',(0.00185038829706693,-0.02565,0.00061527485736214));
#31005=CARTESIAN_POINT('Origin',(9.90111042199066E-15,-0.02565,-1.00514215006786E-14));
#31006=CARTESIAN_POINT('Origin',(0.00196141159488042,-0.02565,0.000652191348814524));
#31007=CARTESIAN_POINT('',(0.00196205693262413,-0.02625,0.000769189569053964));
#31008=CARTESIAN_POINT('Origin',(0.00196141159489036,-0.02625000000001,
0.000652191348804469));
#31009=CARTESIAN_POINT('',(0.00196205693262413,-0.02565,0.000769189569053964));
#31010=CARTESIAN_POINT('',(0.00196205693263408,-0.02565,0.000769189569043909));
#31011=CARTESIAN_POINT('Origin',(0.00196141159489036,-0.02565,0.000652191348804469));
#31012=CARTESIAN_POINT('Origin',(0.00196205693262413,-0.02565,0.000769189569053964));
#31013=CARTESIAN_POINT('',(0.00234426665641354,-0.02625,0.000767081380055257));
#31014=CARTESIAN_POINT('',(0.00234426665642348,-0.02625000000001,0.000767081380045202));
#31015=CARTESIAN_POINT('',(0.00234426665641354,-0.02565,0.000767081380055257));
#31016=CARTESIAN_POINT('',(0.00234426665642348,-0.02565,0.000767081380045202));
#31017=CARTESIAN_POINT('',(0.00234426665642348,-0.02565,0.000767081380045202));
#31018=CARTESIAN_POINT('Origin',(0.00234684800738841,-0.02565,0.00123507426101302));
#31019=CARTESIAN_POINT('',(0.00276099765575108,-0.02625,0.00145302854236826));
#31020=CARTESIAN_POINT('Origin',(0.00234684800739835,-0.02625000000001,
0.00123507426100296));
#31021=CARTESIAN_POINT('',(0.00276099765575108,-0.02565,0.00145302854236826));
#31022=CARTESIAN_POINT('',(0.00276099765576102,-0.02565,0.0014530285423582));
#31023=CARTESIAN_POINT('Origin',(0.00234684800739835,-0.02565,0.00123507426100296));
#31024=CARTESIAN_POINT('Origin',(-4.35815392021282E-17,-0.02565,3.46944695195361E-18));
#31025=CARTESIAN_POINT('',(0.000796650683823533,-0.02625,0.00301657880519694));
#31026=CARTESIAN_POINT('Origin',(9.90123578286685E-15,-0.02625000000001,
-1.00514215006786E-14));
#31027=CARTESIAN_POINT('',(0.000796650683823533,-0.02565,0.00301657880519694));
#31028=CARTESIAN_POINT('',(0.000796650683833588,-0.02565,0.00301657880520689));
#31029=CARTESIAN_POINT('Origin',(9.90111042199066E-15,-0.02565,-1.00514215006786E-14));
#31030=CARTESIAN_POINT('Origin',(0.000716985615441175,-0.02565,0.00271492092467725));
#31031=CARTESIAN_POINT('',(0.000404990361469335,-0.02625,0.00271664182532716));
#31032=CARTESIAN_POINT('Origin',(0.00071698561545123,-0.02625000000001,
0.0027149209246872));
#31033=CARTESIAN_POINT('',(0.000404990361469334,-0.02565,0.00271664182532716));
#31034=CARTESIAN_POINT('',(0.000404990361479389,-0.02565,0.00271664182533711));
#31035=CARTESIAN_POINT('Origin',(0.00071698561545123,-0.02565,0.0027149209246872));
#31036=CARTESIAN_POINT('Origin',(0.000404990361469334,-0.02565,0.00271664182532716));
#31037=CARTESIAN_POINT('',(0.000402900822339103,-0.02625,0.00233781327897642));
#31038=CARTESIAN_POINT('',(0.000402900822349048,-0.02625000000001,0.00233781327896636));
#31039=CARTESIAN_POINT('',(0.000402900822339103,-0.02565,0.00233781327897642));
#31040=CARTESIAN_POINT('',(0.000402900822349048,-0.02565,0.00233781327896636));
#31041=CARTESIAN_POINT('',(0.000402900822349048,-0.02565,0.00233781327896636));
#31042=CARTESIAN_POINT('Origin',(1.29067548743032E-5,-0.02565,0.00233996440478881));
#31043=CARTESIAN_POINT('',(-0.000377087312590497,-0.02625,0.0023421155306012));
#31044=CARTESIAN_POINT('Origin',(1.29067548742481E-5,-0.02625000000001,
0.00233996440477881));
#31045=CARTESIAN_POINT('',(-0.000377087312590497,-0.02565,0.0023421155306012));
#31046=CARTESIAN_POINT('',(-0.000377087312600552,-0.02565,0.00234211553059125));
#31047=CARTESIAN_POINT('Origin',(1.2906754874248E-5,-0.02565,0.00233996440477881));
#31048=CARTESIAN_POINT('Origin',(-0.000377087312590497,-0.02565,0.0023421155306012));
#31049=CARTESIAN_POINT('',(-0.000374997773460266,-0.02625,0.00272094407695195));
#31050=CARTESIAN_POINT('',(-0.000374997773470211,-0.02625000000001,0.00272094407696201));
#31051=CARTESIAN_POINT('',(-0.000374997773460266,-0.02565,0.00272094407695195));
#31052=CARTESIAN_POINT('',(-0.000374997773470211,-0.02565,0.00272094407696201));
#31053=CARTESIAN_POINT('',(-0.000374997773470211,-0.02565,0.00272094407696201));
#31054=CARTESIAN_POINT('Origin',(-0.000686993027432106,-0.02565,0.00272266497760186));
#31055=CARTESIAN_POINT('',(-0.000763325586035669,-0.02625,0.00302518330844651));
#31056=CARTESIAN_POINT('Origin',(-0.000686993027442051,-0.02625000000001,
0.00272266497761192));
#31057=CARTESIAN_POINT('',(-0.000763325586035669,-0.02565,0.00302518330844651));
#31058=CARTESIAN_POINT('',(-0.000763325586045614,-0.02565,0.00302518330845656));
#31059=CARTESIAN_POINT('Origin',(-0.000686993027442051,-0.02565,0.00272266497761192));
#31060=CARTESIAN_POINT('Origin',(-4.35815392021282E-17,-0.02565,3.46944695195361E-18));
#31061=CARTESIAN_POINT('',(-0.00274480094375199,-0.02625,0.00148339737736672));
#31062=CARTESIAN_POINT('Origin',(9.90123578286685E-15,-0.02625000000001,
-1.00514215006786E-14));
#31063=CARTESIAN_POINT('',(-0.00274480094375199,-0.02565,0.00148339737736672));
#31064=CARTESIAN_POINT('',(-0.00274480094376204,-0.02565,0.00148339737735678));
#31065=CARTESIAN_POINT('Origin',(9.90111042199066E-15,-0.02565,-1.00514215006786E-14));
#31066=CARTESIAN_POINT('Origin',(-0.00233308080218919,-0.02565,0.00126088777076171));
#31067=CARTESIAN_POINT('',(-0.00233566215316406,-0.02625,0.000792894889803951));
#31068=CARTESIAN_POINT('Origin',(-0.00233308080219925,-0.02625000000001,
0.00126088777075177));
#31069=CARTESIAN_POINT('',(-0.00233566215316406,-0.02565,0.000792894889803951));
#31070=CARTESIAN_POINT('',(-0.00233566215317412,-0.02565,0.000792894889794006));
#31071=CARTESIAN_POINT('Origin',(-0.00233308080219925,-0.02565,0.00126088777075177));
#31072=CARTESIAN_POINT('Origin',(-0.00233566215316406,-0.02565,0.000792894889803951));
#31073=CARTESIAN_POINT('',(-0.00195345242937466,-0.02625,0.000790786700805244));
#31074=CARTESIAN_POINT('',(-0.00195345242938471,-0.02625000000001,0.000790786700795299));
#31075=CARTESIAN_POINT('',(-0.00195345242937466,-0.02565,0.000790786700805244));
#31076=CARTESIAN_POINT('',(-0.00195345242938471,-0.02565,0.000790786700795299));
#31077=CARTESIAN_POINT('',(-0.00195345242938471,-0.02565,0.000790786700795299));
#31078=CARTESIAN_POINT('Origin',(-0.00195409776711838,-0.02565,0.000673788480565804));
#31079=CARTESIAN_POINT('',(-0.00184348845954563,-0.02625,0.000635649509967742));
#31080=CARTESIAN_POINT('Origin',(-0.00195409776712843,-0.02625000000001,
0.000673788480555859));
#31081=CARTESIAN_POINT('',(-0.00184348845954563,-0.02565,0.000635649509967742));
#31082=CARTESIAN_POINT('',(-0.00184348845955569,-0.02565,0.000635649509957798));
#31083=CARTESIAN_POINT('Origin',(-0.00195409776712843,-0.02565,0.000673788480555859));
#31084=CARTESIAN_POINT('Origin',(-4.35815392021282E-17,-0.02565,3.46944695195361E-18));
#31085=CARTESIAN_POINT('',(-0.00179147958636599,-0.02625,-0.000770130438064942));
#31086=CARTESIAN_POINT('Origin',(9.90123578286685E-15,-0.02625000000001,
-1.00514215006786E-14));
#31087=CARTESIAN_POINT('',(-0.00179147958636599,-0.02565,-0.000770130438064942));
#31088=CARTESIAN_POINT('',(-0.00179147958637604,-0.02565,-0.000770130438074886));
#31089=CARTESIAN_POINT('Origin',(9.90111042199066E-15,-0.02565,-1.00514215006786E-14));
#31090=CARTESIAN_POINT('Origin',(-0.00179147958636599,-0.02565,-0.000770130438064942));
#31091=CARTESIAN_POINT('',(-0.0023805824624172,-0.02625,-0.00239958683686096));
#31092=CARTESIAN_POINT('',(-0.00238058246242725,-0.02625000000001,-0.00239958683687091));
#31093=CARTESIAN_POINT('',(-0.0023805824624172,-0.02565,-0.00239958683686096));
#31094=CARTESIAN_POINT('',(-0.00238058246242725,-0.02565,-0.00239958683687091));
#31095=CARTESIAN_POINT('',(-0.00238058246242725,-0.02565,-0.00239958683687091));
#31096=CARTESIAN_POINT('Origin',(-0.00293073224301609,-0.02565,-0.00220068932831195));
#31097=CARTESIAN_POINT('Origin',(-0.00293073224302614,-0.02625000000001,
-0.0022006893283219));
#31098=CARTESIAN_POINT('Origin',(-0.00293073224302614,-0.02565,-0.0022006893283219));
#31099=CARTESIAN_POINT('Origin',(5.35383428478025E-6,-0.02565,0.000970637606244856));
#31100=CARTESIAN_POINT('Origin',(5.35383428478008E-6,-0.02625,0.000970637606244856));
#31101=CARTESIAN_POINT('',(0.,0.,0.));
#31102=CARTESIAN_POINT('Origin',(0.00360121565085287,-0.008,-0.0126992616256242));
#31103=CARTESIAN_POINT('',(0.00384039707060316,-0.008,-0.0126265137841014));
#31104=CARTESIAN_POINT('',(0.00366942049272508,-0.008,-0.0129397779442914));
#31105=CARTESIAN_POINT('Origin',(0.00360121565086286,-0.00799999999999,
-0.0126992616256342));
#31106=CARTESIAN_POINT('',(0.00366942049272508,-0.024,-0.0129397779442914));
#31107=CARTESIAN_POINT('',(0.00366942049273508,-0.00799999999999,-0.0129397779443014));
#31108=CARTESIAN_POINT('',(0.00384039707060316,-0.024,-0.0126265137841014));
#31109=CARTESIAN_POINT('Origin',(0.00360121565086286,-0.02400000000001,
-0.0126992616256342));
#31110=CARTESIAN_POINT('',(0.00384039707061316,-0.00799999999999,-0.0126265137841114));
#31111=CARTESIAN_POINT('Origin',(-4.44089209850063E-17,-0.008,6.72997231505748E-33));
#31112=CARTESIAN_POINT('',(0.00329207760827845,-0.008,-0.0130408866654485));
#31113=CARTESIAN_POINT('Origin',(-4.44089209850063E-17,-0.00799999999999,
6.72997231505748E-33));
#31114=CARTESIAN_POINT('',(0.00329207760827845,-0.024,-0.0130408866654485));
#31115=CARTESIAN_POINT('',(0.00329207760828845,-0.00799999999999,-0.0130408866654585));
#31116=CARTESIAN_POINT('Origin',(-4.44089209850063E-17,-0.02400000000001,
6.72997231505748E-33));
#31117=CARTESIAN_POINT('Origin',(0.00323088657466734,-0.008,-0.0127984910025219));
#31118=CARTESIAN_POINT('',(0.00298737546828893,-0.008,-0.0128550802335678));
#31119=CARTESIAN_POINT('Origin',(0.00323088657467733,-0.00799999999999,
-0.0127984910025319));
#31120=CARTESIAN_POINT('',(0.00298737546828893,-0.024,-0.0128550802335678));
#31121=CARTESIAN_POINT('',(0.00298737546829892,-0.00799999999999,-0.0128550802335778));
#31122=CARTESIAN_POINT('Origin',(0.00323088657467733,-0.02400000000001,
-0.0127984910025319));
#31123=CARTESIAN_POINT('Origin',(0.00294264001438597,-0.008,-0.0126625775316771));
#31124=CARTESIAN_POINT('',(0.00294264001438597,-0.008,-0.0126625775316771));
#31125=CARTESIAN_POINT('',(0.00291295831081407,-0.00799999999999,-0.0125348531511851));
#31126=CARTESIAN_POINT('',(0.00294264001438597,-0.024,-0.0126625775316771));
#31127=CARTESIAN_POINT('',(0.00294264001439597,-0.016,-0.0126625775316871));
#31128=CARTESIAN_POINT('',(0.00291295831081407,-0.02400000000001,-0.0125348531511851));
#31129=CARTESIAN_POINT('Origin',(0.00191282048773806,-0.008,-0.0130606706482359));
#31130=CARTESIAN_POINT('',(0.00215945117603179,-0.008,-0.0130197646145518));
#31131=CARTESIAN_POINT('',(0.00194904814849068,-0.008,-0.0133080318347555));
#31132=CARTESIAN_POINT('Origin',(0.00191282048774806,-0.00799999999999,
-0.0130606706482459));
#31133=CARTESIAN_POINT('',(0.00194904814849068,-0.024,-0.0133080318347555));
#31134=CARTESIAN_POINT('',(0.00194904814850068,-0.00799999999999,-0.0133080318347655));
#31135=CARTESIAN_POINT('',(0.00215945117603179,-0.024,-0.0130197646145518));
#31136=CARTESIAN_POINT('Origin',(0.00191282048774806,-0.02400000000001,
-0.0130606706482459));
#31137=CARTESIAN_POINT('',(0.0021594511760418,-0.00799999999999,-0.0130197646145618));
#31138=CARTESIAN_POINT('Origin',(-4.44089209850063E-17,-0.008,6.72997231505748E-33));
#31139=CARTESIAN_POINT('',(0.00156173614835723,-0.008,-0.0133590224269186));
#31140=CARTESIAN_POINT('Origin',(-4.44089209850063E-17,-0.00799999999999,
6.72997231505748E-33));
#31141=CARTESIAN_POINT('',(0.00156173614835723,-0.024,-0.0133590224269186));
#31142=CARTESIAN_POINT('',(0.00156173614836722,-0.00799999999999,-0.0133590224269286));
#31143=CARTESIAN_POINT('Origin',(-4.44089209850063E-17,-0.02400000000001,
6.72997231505748E-33));
#31144=CARTESIAN_POINT('Origin',(0.00153270759541378,-0.008,-0.0131107134598755));
#31145=CARTESIAN_POINT('',(0.00128389338345838,-0.008,-0.0131350339847262));
#31146=CARTESIAN_POINT('Origin',(0.00153270759542378,-0.00799999999999,
-0.0131107134598855));
#31147=CARTESIAN_POINT('',(0.00128389338345838,-0.024,-0.0131350339847262));
#31148=CARTESIAN_POINT('',(0.00128389338346838,-0.00799999999999,-0.0131350339847362));
#31149=CARTESIAN_POINT('Origin',(0.00153270759542378,-0.02400000000001,
-0.0131107134598855));
#31150=CARTESIAN_POINT('Origin',(0.00126466729223494,-0.008,-0.0129383390216809));
#31151=CARTESIAN_POINT('',(0.00126466729223494,-0.008,-0.0129383390216809));
#31152=CARTESIAN_POINT('',(0.00126540384839637,-0.00799999999999,-0.0129458744527519));
#31153=CARTESIAN_POINT('',(0.00126466729223494,-0.024,-0.0129383390216809));
#31154=CARTESIAN_POINT('',(0.00126466729224494,-0.016,-0.0129383390216909));
#31155=CARTESIAN_POINT('',(0.00126540384839637,-0.02400000000001,-0.0129458744527519));
#31156=CARTESIAN_POINT('Origin',(0.000191696435744033,-0.008,-0.0131986079749541));
#31157=CARTESIAN_POINT('',(0.000441556473125542,-0.008,-0.0131902436626865));
#31158=CARTESIAN_POINT('',(0.000195327050057368,-0.008,-0.0134485816108434));
#31159=CARTESIAN_POINT('Origin',(0.000191696435754032,-0.00799999999999,
-0.0131986079749641));
#31160=CARTESIAN_POINT('',(0.000195327050057368,-0.024,-0.0134485816108434));
#31161=CARTESIAN_POINT('',(0.000195327050067368,-0.00799999999999,-0.0134485816108534));
#31162=CARTESIAN_POINT('',(0.000441556473125542,-0.024,-0.0131902436626865));
#31163=CARTESIAN_POINT('Origin',(0.000191696435754032,-0.02400000000001,
-0.0131986079749641));
#31164=CARTESIAN_POINT('',(0.000441556473135542,-0.00799999999999,-0.0131902436626965));
#31165=CARTESIAN_POINT('Origin',(-4.44089209850063E-17,-0.008,6.72997231505748E-33));
#31166=CARTESIAN_POINT('',(-0.00019532705005746,-0.008,-0.0134485816108434));
#31167=CARTESIAN_POINT('Origin',(-4.44089209850063E-17,-0.00799999999999,
6.72997231505748E-33));
#31168=CARTESIAN_POINT('',(-0.00019532705005746,-0.024,-0.0134485816108434));
#31169=CARTESIAN_POINT('',(-0.00019532705006746,-0.00799999999999,-0.0134485816108534));
#31170=CARTESIAN_POINT('Origin',(-4.44089209850063E-17,-0.02400000000001,
6.72997231505748E-33));
#31171=CARTESIAN_POINT('Origin',(-0.000191696435744125,-0.008,-0.0131986079749541));
#31172=CARTESIAN_POINT('',(-0.000441556473125634,-0.008,-0.0131902436626865));
#31173=CARTESIAN_POINT('Origin',(-0.000191696435754125,-0.00799999999999,
-0.0131986079749641));
#31174=CARTESIAN_POINT('',(-0.000441556473125634,-0.024,-0.0131902436626865));
#31175=CARTESIAN_POINT('',(-0.000441556473135633,-0.00799999999999,-0.0131902436626965));
#31176=CARTESIAN_POINT('Origin',(-0.000191696435754125,-0.02400000000001,
-0.0131986079749641));
#31177=CARTESIAN_POINT('Origin',(-0.000434944237918262,-0.008,-0.0129927219438385));
#31178=CARTESIAN_POINT('',(-0.000434944237918262,-0.008,-0.0129927219438385));
#31179=CARTESIAN_POINT('',(-0.000436112706129081,-0.00799999999999,-0.0130276266077339));
#31180=CARTESIAN_POINT('',(-0.000434944237918262,-0.024,-0.0129927219438385));
#31181=CARTESIAN_POINT('',(-0.000434944237928261,-0.016,-0.0129927219438485));
#31182=CARTESIAN_POINT('',(-0.000436112706129081,-0.02400000000001,-0.0130276266077339));
#31183=CARTESIAN_POINT('Origin',(-0.00153270759541388,-0.008,-0.0131107134598755));
#31184=CARTESIAN_POINT('',(-0.00128389338345847,-0.008,-0.0131350339847262));
#31185=CARTESIAN_POINT('',(-0.00156173614835732,-0.008,-0.0133590224269186));
#31186=CARTESIAN_POINT('Origin',(-0.00153270759542387,-0.00799999999999,
-0.0131107134598855));
#31187=CARTESIAN_POINT('',(-0.00156173614835732,-0.024,-0.0133590224269186));
#31188=CARTESIAN_POINT('',(-0.00156173614836731,-0.00799999999999,-0.0133590224269286));
#31189=CARTESIAN_POINT('',(-0.00128389338345847,-0.024,-0.0131350339847262));
#31190=CARTESIAN_POINT('Origin',(-0.00153270759542387,-0.02400000000001,
-0.0131107134598855));
#31191=CARTESIAN_POINT('',(-0.00128389338346847,-0.00799999999999,-0.0131350339847362));
#31192=CARTESIAN_POINT('Origin',(-4.44089209850063E-17,-0.008,6.72997231505748E-33));
#31193=CARTESIAN_POINT('',(-0.00194904814849077,-0.008,-0.0133080318347555));
#31194=CARTESIAN_POINT('Origin',(-4.44089209850063E-17,-0.00799999999999,
6.72997231505748E-33));
#31195=CARTESIAN_POINT('',(-0.00194904814849077,-0.024,-0.0133080318347555));
#31196=CARTESIAN_POINT('',(-0.00194904814850077,-0.00799999999999,-0.0133080318347655));
#31197=CARTESIAN_POINT('Origin',(-4.44089209850063E-17,-0.02400000000001,
6.72997231505748E-33));
#31198=CARTESIAN_POINT('Origin',(-0.00191282048773815,-0.008,-0.0130606706482359));
#31199=CARTESIAN_POINT('',(-0.00215945117603188,-0.008,-0.0130197646145518));
#31200=CARTESIAN_POINT('Origin',(-0.00191282048774815,-0.00799999999999,
-0.0130606706482459));
#31201=CARTESIAN_POINT('',(-0.00215945117603188,-0.024,-0.0130197646145518));
#31202=CARTESIAN_POINT('',(-0.00215945117604188,-0.00799999999999,-0.0130197646145618));
#31203=CARTESIAN_POINT('Origin',(-0.00191282048774815,-0.02400000000001,
-0.0130606706482459));
#31204=CARTESIAN_POINT('Origin',(-0.00212711375157135,-0.008,-0.0128247957912739));
#31205=CARTESIAN_POINT('',(-0.00212711375157135,-0.008,-0.0128247957912739));
#31206=CARTESIAN_POINT('',(-0.00211900825769018,-0.00799999999999,-0.0127759261415696));
#31207=CARTESIAN_POINT('',(-0.00212711375157135,-0.024,-0.0128247957912739));
#31208=CARTESIAN_POINT('',(-0.00212711375158135,-0.016,-0.0128247957912839));
#31209=CARTESIAN_POINT('',(-0.00211900825769018,-0.02400000000001,-0.0127759261415696));
#31210=CARTESIAN_POINT('Origin',(-0.00323088657466742,-0.008,-0.0127984910025219));
#31211=CARTESIAN_POINT('',(-0.00298737546828901,-0.008,-0.0128550802335678));
#31212=CARTESIAN_POINT('',(-0.00329207760827854,-0.008,-0.0130408866654485));
#31213=CARTESIAN_POINT('Origin',(-0.00323088657467743,-0.00799999999999,
-0.0127984910025319));
#31214=CARTESIAN_POINT('',(-0.00329207760827854,-0.024,-0.0130408866654485));
#31215=CARTESIAN_POINT('',(-0.00329207760828854,-0.00799999999999,-0.0130408866654585));
#31216=CARTESIAN_POINT('',(-0.00298737546828901,-0.024,-0.0128550802335678));
#31217=CARTESIAN_POINT('Origin',(-0.00323088657467743,-0.02400000000001,
-0.0127984910025319));
#31218=CARTESIAN_POINT('',(-0.00298737546829902,-0.00799999999999,-0.0128550802335778));
#31219=CARTESIAN_POINT('Origin',(-4.44089209850063E-17,-0.008,6.72997231505748E-33));
#31220=CARTESIAN_POINT('',(-0.00366942049272517,-0.008,-0.0129397779442914));
#31221=CARTESIAN_POINT('Origin',(-4.44089209850063E-17,-0.00799999999999,
6.72997231505748E-33));
#31222=CARTESIAN_POINT('',(-0.00366942049272517,-0.024,-0.0129397779442914));
#31223=CARTESIAN_POINT('',(-0.00366942049273517,-0.00799999999999,-0.0129397779443014));
#31224=CARTESIAN_POINT('Origin',(-4.44089209850063E-17,-0.02400000000001,
6.72997231505748E-33));
#31225=CARTESIAN_POINT('Origin',(-0.00360121565085296,-0.008,-0.0126992616256242));
#31226=CARTESIAN_POINT('',(-0.00384039707060325,-0.008,-0.0126265137841014));
#31227=CARTESIAN_POINT('Origin',(-0.00360121565086297,-0.00799999999999,
-0.0126992616256342));
#31228=CARTESIAN_POINT('',(-0.00384039707060325,-0.024,-0.0126265137841014));
#31229=CARTESIAN_POINT('',(-0.00384039707061325,-0.00799999999999,-0.0126265137841114));
#31230=CARTESIAN_POINT('Origin',(-0.00360121565086297,-0.02400000000001,
-0.0126992616256342));
#31231=CARTESIAN_POINT('Origin',(-0.0037828877591877,-0.008,-0.0124374338270155));
#31232=CARTESIAN_POINT('',(-0.0037828877591877,-0.008,-0.0124374338270155));
#31233=CARTESIAN_POINT('',(-0.00371177878877267,-0.00799999999999,-0.0122036407116943));
#31234=CARTESIAN_POINT('',(-0.0037828877591877,-0.024,-0.0124374338270155));
#31235=CARTESIAN_POINT('',(-0.00378288775919771,-0.016,-0.0124374338270255));
#31236=CARTESIAN_POINT('',(-0.00371177878877267,-0.02400000000001,-0.0122036407116943));
#31237=CARTESIAN_POINT('Origin',(-0.00304450063026865,-0.008,-0.0131008975231583));
#31238=CARTESIAN_POINT('',(-0.00294264001438606,-0.024,-0.0126625775316771));
#31239=CARTESIAN_POINT('',(-0.00296388861875547,-0.02400000000001,-0.0127540131469256));
#31240=CARTESIAN_POINT('',(-0.00294264001438606,-0.008,-0.0126625775316771));
#31241=CARTESIAN_POINT('',(-0.00294264001439606,-0.016,-0.0126625775316871));
#31242=CARTESIAN_POINT('',(-0.00296388861875547,-0.00799999999999,-0.0127540131469256));
#31243=CARTESIAN_POINT('Origin',(-0.00130844423696623,-0.008,-0.0133862046032006));
#31244=CARTESIAN_POINT('',(-0.00126466729223502,-0.024,-0.0129383390216809));
#31245=CARTESIAN_POINT('',(-0.00128729232076206,-0.02400000000001,-0.0131698072435117));
#31246=CARTESIAN_POINT('',(-0.00126466729223502,-0.008,-0.0129383390216809));
#31247=CARTESIAN_POINT('',(-0.00126466729224502,-0.016,-0.0129383390216909));
#31248=CARTESIAN_POINT('',(-0.00128729232076206,-0.00799999999999,-0.0131698072435117));
#31249=CARTESIAN_POINT('Origin',(0.00220074461220257,-0.008,-0.0132687310302026));
#31250=CARTESIAN_POINT('',(0.00212711375157125,-0.024,-0.0128247957912739));
#31251=CARTESIAN_POINT('',(0.00215582368800574,-0.02400000000001,-0.0129978937610339));
#31252=CARTESIAN_POINT('',(0.00212711375157125,-0.008,-0.0128247957912739));
#31253=CARTESIAN_POINT('',(0.00212711375158126,-0.016,-0.0128247957912839));
#31254=CARTESIAN_POINT('',(0.00215582368800574,-0.00799999999999,-0.0129978937610339));
#31255=CARTESIAN_POINT('Origin',(0.00391383387392873,-0.008,-0.012867960382566));
#31256=CARTESIAN_POINT('',(0.00378288775918762,-0.024,-0.0124374338270155));
#31257=CARTESIAN_POINT('',(0.00377725184614313,-0.02400000000001,-0.0124189039894696));
#31258=CARTESIAN_POINT('',(0.00378288775918762,-0.008,-0.0124374338270155));
#31259=CARTESIAN_POINT('',(0.00378288775919761,-0.016,-0.0124374338270255));
#31260=CARTESIAN_POINT('',(0.00377725184614313,-0.00799999999999,-0.0124189039894696));
#31261=CARTESIAN_POINT('Origin',(-4.44089209850063E-17,-0.016,6.72997231505748E-33));
#31262=CARTESIAN_POINT('',(-0.00433948917003907,-0.008,-0.0122543393841983));
#31263=CARTESIAN_POINT('Origin',(-4.44089209850063E-17,-0.00799999999999,
6.72997231505748E-33));
#31264=CARTESIAN_POINT('',(-0.00433948917003907,-0.024,-0.0122543393841983));
#31265=CARTESIAN_POINT('',(-0.00433948917004907,-0.016,-0.0122543393842083));
#31266=CARTESIAN_POINT('Origin',(-4.44089209850063E-17,-0.02400000000001,
6.72997231505748E-33));
#31267=CARTESIAN_POINT('Origin',(-4.44089209850063E-17,-0.016,6.72997231505748E-33));
#31268=CARTESIAN_POINT('Origin',(-4.44089209850063E-17,-0.02400000000001,
6.72997231505748E-33));
#31269=CARTESIAN_POINT('Origin',(-4.44089209850063E-17,-0.00799999999999,
6.72997231505748E-33));
#31270=CARTESIAN_POINT('Origin',(-4.57966997657877E-17,-0.024,-0.0130771696920992));
#31271=CARTESIAN_POINT('',(-0.00463991534334946,-0.024,-0.0131027167261813));
#31272=CARTESIAN_POINT('',(-0.00463991534335947,-0.02400000000001,-0.0131027167261913));
#31273=CARTESIAN_POINT('',(0.00463991534334938,-0.024,-0.0131027167261813));
#31274=CARTESIAN_POINT('Origin',(-4.44089209850063E-17,-0.02400000000001,
6.72997231505748E-33));
#31275=CARTESIAN_POINT('',(0.00433948917003898,-0.024,-0.0122543393841983));
#31276=CARTESIAN_POINT('',(0.00433948917004898,-0.02400000000001,-0.0122543393842083));
#31277=CARTESIAN_POINT('Origin',(-4.44089209850063E-17,-0.02400000000001,
6.72997231505748E-33));
#31278=CARTESIAN_POINT('Origin',(-4.44089209850063E-17,-0.02400000000001,
6.72997231505748E-33));
#31279=CARTESIAN_POINT('',(0.00043494423791817,-0.024,-0.0129927219438385));
#31280=CARTESIAN_POINT('Origin',(-4.44089209850063E-17,-0.02400000000001,
6.72997231505748E-33));
#31281=CARTESIAN_POINT('',(0.000443640587169881,-0.02400000000001,-0.0132525006413773));
#31282=CARTESIAN_POINT('Origin',(-4.44089209850063E-17,-0.02400000000001,
6.72997231505748E-33));
#31283=CARTESIAN_POINT('Origin',(-4.44089209850063E-17,-0.016,6.72997231505748E-33));
#31284=CARTESIAN_POINT('',(0.00043494423791817,-0.008,-0.0129927219438385));
#31285=CARTESIAN_POINT('Origin',(-4.44089209850063E-17,-0.00799999999999,
6.72997231505748E-33));
#31286=CARTESIAN_POINT('',(0.00043494423792817,-0.016,-0.0129927219438485));
#31287=CARTESIAN_POINT('Origin',(-4.44089209850063E-17,-0.016,6.72997231505748E-33));
#31288=CARTESIAN_POINT('',(0.00433948917003898,-0.008,-0.0122543393841983));
#31289=CARTESIAN_POINT('',(0.00433948917004898,-0.016,-0.0122543393842083));
#31290=CARTESIAN_POINT('Origin',(-4.44089209850063E-17,-0.00799999999999,
6.72997231505748E-33));
#31291=CARTESIAN_POINT('Origin',(0.000449999999999955,-0.008,-0.0134424700111252));
#31292=CARTESIAN_POINT('',(0.000443640587169881,-0.00799999999999,-0.0132525006413773));
#31293=CARTESIAN_POINT('Origin',(-4.44089209850063E-17,-0.016,6.72997231505748E-33));
#31294=CARTESIAN_POINT('Origin',(-4.44089209850063E-17,-0.00799999999999,
6.72997231505748E-33));
#31295=CARTESIAN_POINT('Origin',(-0.00463991534334946,-0.016,-0.0131027167261813));
#31296=CARTESIAN_POINT('',(-0.00463991534334946,-0.008,-0.0131027167261813));
#31297=CARTESIAN_POINT('',(-0.00463991534335947,-0.00799999999999,-0.0131027167261913));
#31298=CARTESIAN_POINT('',(-0.00463991534335947,-0.016,-0.0131027167261913));
#31299=CARTESIAN_POINT('Origin',(-4.44089209850063E-17,-0.016,6.72997231505748E-33));
#31300=CARTESIAN_POINT('',(0.00463991534334938,-0.008,-0.0131027167261813));
#31301=CARTESIAN_POINT('Origin',(-4.44089209850063E-17,-0.00799999999999,
6.72997231505748E-33));
#31302=CARTESIAN_POINT('',(0.00463991534335938,-0.016,-0.0131027167261913));
#31303=CARTESIAN_POINT('Origin',(0.00433948917003898,-0.016,-0.0122543393841983));
#31304=CARTESIAN_POINT('',(0.00433948917004898,-0.00799999999999,-0.0122543393842083));
#31305=CARTESIAN_POINT('Origin',(-4.44089209850063E-17,-0.016,6.72997231505748E-33));
#31306=CARTESIAN_POINT('Origin',(-4.44089209850063E-17,-0.00799999999999,
6.72997231505748E-33));
#31307=CARTESIAN_POINT('Origin',(-4.57966997657877E-17,-0.008,-0.0130771696920992));
#31308=CARTESIAN_POINT('',(0.,0.,0.));
#31309=CARTESIAN_POINT('Origin',(0.0129631448730721,-0.024,0.0191500000000096));
#31310=CARTESIAN_POINT('',(0.014084281726958,-0.008,0.0208062162162298));
#31311=CARTESIAN_POINT('',(0.0131664441683726,-0.00800000000001,0.0211396405194357));
#31312=CARTESIAN_POINT('Origin',(0.0129631448730721,-0.008,0.0191500000000096));
#31313=CARTESIAN_POINT('',(0.014084281726958,-5.52435218316827E-5,0.0208062162162298));
#31314=CARTESIAN_POINT('',(0.014084281726958,-0.024,0.0208062162162298));
#31315=CARTESIAN_POINT('',(0.0137123694638326,-0.0002499619237991,0.0210043631016193));
#31316=CARTESIAN_POINT('Origin',(0.0129631448730721,0.00157231562097569,
0.0191500000000096));
#31317=CARTESIAN_POINT('Origin',(0.0129631448730721,0.105986429016355,0.0191500000000096));
#31318=CARTESIAN_POINT('Origin',(-1.00275343584144E-14,-0.024,9.9475983006414E-15));
#31319=CARTESIAN_POINT('',(0.020806216216238,-0.008,0.0140842817269634));
#31320=CARTESIAN_POINT('Origin',(-1.00275343584144E-14,-0.008,9.9475983006414E-15));
#31321=CARTESIAN_POINT('',(0.020806216216238,-5.52435218397962E-5,0.0140842817269634));
#31322=CARTESIAN_POINT('',(0.020806216216238,-0.024,0.0140842817269634));
#31323=CARTESIAN_POINT('',(0.02075000000001,0.,0.014166973035935));
#31324=CARTESIAN_POINT('Origin',(-1.00275343584144E-14,0.0203909682096601,
9.9475983006414E-15));
#31325=CARTESIAN_POINT('',(0.0141669730359443,0.,0.02075000000001));
#31326=CARTESIAN_POINT('Origin',(-1.00275343584144E-14,0.,9.9475983006414E-15));
#31327=CARTESIAN_POINT('Origin',(-1.00275343584144E-14,0.0203909682096408,
9.9475983006414E-15));
#31328=CARTESIAN_POINT('Origin',(-0.0191500000000098,-0.024,0.0129631448730722));
#31329=CARTESIAN_POINT('',(-0.0208062162162391,-0.008,0.0140842817269642));
#31330=CARTESIAN_POINT('',(-0.0211396405194357,-0.00800000000001,0.013166444168483));
#31331=CARTESIAN_POINT('Origin',(-0.0191500000000098,-0.008,0.0129631448730722));
#31332=CARTESIAN_POINT('',(-0.0208062162162391,-5.52435218408842E-5,0.0140842817269642));
#31333=CARTESIAN_POINT('',(-0.0208062162162391,-0.024,0.0140842817269642));
#31334=CARTESIAN_POINT('',(-0.0210043631016193,-0.0002499619237991,0.0137123694638626));
#31335=CARTESIAN_POINT('Origin',(-0.0191500000000098,0.00157231562097551,
0.0129631448730722));
#31336=CARTESIAN_POINT('Origin',(-0.0191500000000098,0.105986429016344,
0.0129631448730722));
#31337=CARTESIAN_POINT('Origin',(-1.00275343584144E-14,-0.024,9.9475983006414E-15));
#31338=CARTESIAN_POINT('',(-0.0140842817269636,-0.008,0.0208062162162381));
#31339=CARTESIAN_POINT('Origin',(-1.00275343584144E-14,-0.008,9.9475983006414E-15));
#31340=CARTESIAN_POINT('',(-0.0140842817269636,-5.52435218398184E-5,0.0208062162162381));
#31341=CARTESIAN_POINT('',(-0.0140842817269636,-0.024,0.0208062162162381));
#31342=CARTESIAN_POINT('',(-0.0141669730359351,0.,0.02075000000001));
#31343=CARTESIAN_POINT('Origin',(-1.00275343584144E-14,0.0203909682096408,
9.9475983006414E-15));
#31344=CARTESIAN_POINT('',(-0.02075000000001,0.,0.0141669730359352));
#31345=CARTESIAN_POINT('Origin',(-1.00275343584144E-14,0.,9.9475983006414E-15));
#31346=CARTESIAN_POINT('Origin',(-1.00275343584144E-14,0.0203909682096408,
9.9475983006414E-15));
#31347=CARTESIAN_POINT('Origin',(-0.0129631448730721,-0.024,-0.0191500000000097));
#31348=CARTESIAN_POINT('',(-0.014084281726955,-0.008,-0.0208062162162255));
#31349=CARTESIAN_POINT('',(-0.0131664441683213,-0.00800000000001,-0.0211396405194357));
#31350=CARTESIAN_POINT('Origin',(-0.0129631448730721,-0.008,-0.0191500000000097));
#31351=CARTESIAN_POINT('',(-0.014084281726955,-5.52435218274594E-5,-0.0208062162162255));
#31352=CARTESIAN_POINT('',(-0.014084281726955,-0.024,-0.0208062162162255));
#31353=CARTESIAN_POINT('',(-0.0137123694638187,-0.0002499619237991,-0.0210043631016193));
#31354=CARTESIAN_POINT('Origin',(-0.0129631448730721,0.00157231562097559,
-0.0191500000000097));
#31355=CARTESIAN_POINT('Origin',(-0.0129631448730721,0.105986429016349,
-0.0191500000000097));
#31356=CARTESIAN_POINT('Origin',(-1.00275343584144E-14,-0.024,9.9475983006414E-15));
#31357=CARTESIAN_POINT('',(-0.0208062162162194,-0.008,-0.0140842817269509));
#31358=CARTESIAN_POINT('Origin',(-1.00275343584144E-14,-0.008,9.9475983006414E-15));
#31359=CARTESIAN_POINT('',(-0.0208062162162194,-5.52435218215264E-5,-0.0140842817269509));
#31360=CARTESIAN_POINT('',(-0.0208062162162194,-0.024,-0.0140842817269509));
#31361=CARTESIAN_POINT('',(-0.02075000000001,0.,-0.0141669730359175));
#31362=CARTESIAN_POINT('Origin',(-1.00275343584144E-14,0.0203909682096408,
9.9475983006414E-15));
#31363=CARTESIAN_POINT('',(-0.0141669730359082,0.,-0.02075000000001));
#31364=CARTESIAN_POINT('Origin',(-1.00275343584144E-14,0.,9.9475983006414E-15));
#31365=CARTESIAN_POINT('Origin',(-1.00275343584144E-14,0.0203909682096604,
9.9475983006414E-15));
#31366=CARTESIAN_POINT('Origin',(0.01915000000001,-0.024,-0.0129631448730722));
#31367=CARTESIAN_POINT('',(0.0208062162162161,-0.008,-0.0140842817269487));
#31368=CARTESIAN_POINT('',(0.0211396405194357,-0.00800000000001,-0.0131664441682106));
#31369=CARTESIAN_POINT('Origin',(0.01915000000001,-0.008,-0.0129631448730722));
#31370=CARTESIAN_POINT('',(0.0208062162162161,-5.52435218182845E-5,-0.0140842817269487));
#31371=CARTESIAN_POINT('',(0.0208062162162161,-0.024,-0.0140842817269487));
#31372=CARTESIAN_POINT('',(0.0210043631016193,-0.0002499619237991,-0.0137123694637886));
#31373=CARTESIAN_POINT('Origin',(0.01915000000001,0.00157231562097526,-0.0129631448730722));
#31374=CARTESIAN_POINT('Origin',(0.01915000000001,0.105986429016332,-0.0129631448730722));
#31375=CARTESIAN_POINT('Origin',(-1.00275343584144E-14,-0.024,9.9475983006414E-15));
#31376=CARTESIAN_POINT('',(0.0140842817269635,-0.008,-0.0208062162162381));
#31377=CARTESIAN_POINT('Origin',(-1.00275343584144E-14,-0.008,9.9475983006414E-15));
#31378=CARTESIAN_POINT('',(0.0140842817269635,-5.52435218398539E-5,-0.0208062162162381));
#31379=CARTESIAN_POINT('',(0.0140842817269635,-0.024,-0.0208062162162381));
#31380=CARTESIAN_POINT('',(0.0141669730358881,0.,-0.02075000000001));
#31381=CARTESIAN_POINT('Origin',(-1.00275343584144E-14,0.0203909682096604,
9.9475983006414E-15));
#31382=CARTESIAN_POINT('',(0.02075000000001,0.,-0.0141669730358881));
#31383=CARTESIAN_POINT('Origin',(-1.00275343584144E-14,0.,9.9475983006414E-15));
#31384=CARTESIAN_POINT('Origin',(-1.00275343584144E-14,0.0203909682096601,
9.9475983006414E-15));
#31385=CARTESIAN_POINT('Origin',(0.01915000000001,-0.024,0.0129631448730722));
#31386=CARTESIAN_POINT('',(0.0211396405194357,-0.00800000000001,0.0131664441682491));
#31387=CARTESIAN_POINT('Origin',(0.01915000000001,-0.008,0.0129631448730722));
#31388=CARTESIAN_POINT('',(0.0210043631016193,-0.0002499619237991,0.0137123694637991));
#31389=CARTESIAN_POINT('Origin',(0.01915000000001,0.105986429016333,0.0129631448730722));
#31390=CARTESIAN_POINT('Origin',(0.01915000000001,0.00157231562097527,0.0129631448730722));
#31391=CARTESIAN_POINT('Origin',(-0.0129631448730724,-0.024,0.0191500000000103));
#31392=CARTESIAN_POINT('',(-0.0131664441682495,-0.00800000000001,0.0211396405194357));
#31393=CARTESIAN_POINT('Origin',(-0.0129631448730724,-0.008,0.0191500000000103));
#31394=CARTESIAN_POINT('',(-0.0137123694637993,-0.0002499619237991,0.0210043631016193));
#31395=CARTESIAN_POINT('Origin',(-0.0129631448730724,0.105986429016316,
0.0191500000000103));
#31396=CARTESIAN_POINT('Origin',(-0.0129631448730724,0.00157231562097503,
0.0191500000000103));
#31397=CARTESIAN_POINT('Origin',(-0.01915000000001,-0.024,-0.0129631448730723));
#31398=CARTESIAN_POINT('',(-0.0211396405194357,-0.00800000000001,-0.0131664441682492));
#31399=CARTESIAN_POINT('Origin',(-0.01915000000001,-0.008,-0.0129631448730723));
#31400=CARTESIAN_POINT('',(-0.0210043631016193,-0.0002499619237991,-0.0137123694637992));
#31401=CARTESIAN_POINT('Origin',(-0.01915000000001,0.105986429016332,-0.0129631448730723));
#31402=CARTESIAN_POINT('Origin',(-0.01915000000001,0.00157231562097529,
-0.0129631448730723));
#31403=CARTESIAN_POINT('Origin',(0.012963144873072,-0.024,-0.0191500000000096));
#31404=CARTESIAN_POINT('',(0.0131664441684711,-0.00800000000001,-0.0211396405194357));
#31405=CARTESIAN_POINT('Origin',(0.012963144873072,-0.008,-0.0191500000000096));
#31406=CARTESIAN_POINT('',(0.0137123694638593,-0.0002499619237991,-0.0210043631016193));
#31407=CARTESIAN_POINT('Origin',(0.012963144873072,0.105986429016355,-0.0191500000000096));
#31408=CARTESIAN_POINT('Origin',(0.012963144873072,0.00157231562097569,
-0.0191500000000096));
#31409=CARTESIAN_POINT('Origin',(-0.016,0.,0.021));
#31410=CARTESIAN_POINT('',(-0.00800000000001,-0.000249961923799098,0.0210043631016193));
#31411=CARTESIAN_POINT('',(-0.01600000000001,-0.00800000000001,0.0211396405194357));
#31412=CARTESIAN_POINT('Origin',(-0.008,-0.000124980961894549,0.0208771815508047));
#31413=CARTESIAN_POINT('',(-0.00800000000001,0.,0.02075000000001));
#31414=CARTESIAN_POINT('Origin',(-0.021,0.,-0.016));
#31415=CARTESIAN_POINT('',(-0.0210043631016193,-0.000249961923799098,-0.00800000000001));
#31416=CARTESIAN_POINT('',(-0.0211396405194357,-0.00800000000001,-0.01600000000001));
#31417=CARTESIAN_POINT('Origin',(-0.0208771815508047,-0.000124980961894549,
-0.008));
#31418=CARTESIAN_POINT('',(-0.02075000000001,0.,-0.00800000000001));
#31419=CARTESIAN_POINT('Origin',(0.016,0.,-0.021));
#31420=CARTESIAN_POINT('',(0.00800000000001,-0.000249961923799098,-0.0210043631016193));
#31421=CARTESIAN_POINT('',(0.01600000000001,-0.00800000000001,-0.0211396405194357));
#31422=CARTESIAN_POINT('Origin',(2.22044604925031E-18,-0.008,0.));
#31423=CARTESIAN_POINT('',(0.0211396405194357,-0.00800000000001,0.01600000000001));
#31424=CARTESIAN_POINT('',(0.00807716446627536,-0.008,0.0195));
#31425=CARTESIAN_POINT('',(0.0195,-0.008,0.00807716446627536));
#31426=CARTESIAN_POINT('',(0.0109328733497165,-0.00800000000001,0.0166442911165789));
#31427=CARTESIAN_POINT('',(0.0195,-0.008,-0.00807716446627536));
#31428=CARTESIAN_POINT('',(0.01950000000001,-0.00800000000001,0.00403858223314768));
#31429=CARTESIAN_POINT('',(0.00807716446627536,-0.008,-0.0195));
#31430=CARTESIAN_POINT('',(0.0166442911165789,-0.00800000000001,-0.0109328733497165));
#31431=CARTESIAN_POINT('',(-0.00807716446627536,-0.008,-0.0195));
#31432=CARTESIAN_POINT('',(0.00403858223314768,-0.00800000000001,-0.01950000000001));
#31433=CARTESIAN_POINT('',(-0.0195,-0.008,-0.00807716446627536));
#31434=CARTESIAN_POINT('',(-0.0109328733497165,-0.00800000000001,-0.0166442911165788));
#31435=CARTESIAN_POINT('',(-0.0195,-0.008,0.00807716446627536));
#31436=CARTESIAN_POINT('',(-0.01950000000001,-0.00800000000001,-0.00403858223314768));
#31437=CARTESIAN_POINT('',(-0.00807716446627536,-0.008,0.0195));
#31438=CARTESIAN_POINT('',(-0.0166442911165788,-0.00800000000001,0.0109328733497165));
#31439=CARTESIAN_POINT('',(-0.00403858223314768,-0.00800000000001,0.01950000000001));
#31440=CARTESIAN_POINT('',(-0.0167295,-0.00800000000001,0.0155));
#31441=CARTESIAN_POINT('Origin',(-0.01550000000001,-0.00800000000001,0.01550000000001));
#31442=CARTESIAN_POINT('',(0.0142705,-0.00800000000001,-0.0155));
#31443=CARTESIAN_POINT('Origin',(0.01550000000001,-0.00800000000001,-0.01550000000001));
#31444=CARTESIAN_POINT('',(-0.0167295,-0.00800000000001,-0.0155));
#31445=CARTESIAN_POINT('Origin',(-0.01550000000001,-0.00800000000001,-0.01550000000001));
#31446=CARTESIAN_POINT('',(0.0142705,-0.00800000000001,0.0155));
#31447=CARTESIAN_POINT('Origin',(0.01550000000001,-0.00800000000001,0.01550000000001));
#31448=CARTESIAN_POINT('Origin',(0.008,-0.000124980961894549,-0.0208771815508047));
#31449=CARTESIAN_POINT('',(0.00800000000001,0.,-0.02075000000001));
#31450=CARTESIAN_POINT('Origin',(2.22044604925031E-18,0.,0.));
#31451=CARTESIAN_POINT('',(0.02075000000001,0.,0.00800000000001));
#31452=CARTESIAN_POINT('',(0.0142705,0.,0.0155));
#31453=CARTESIAN_POINT('Origin',(0.01550000000001,0.,0.01550000000001));
#31454=CARTESIAN_POINT('',(-0.0167295,0.,-0.0155));
#31455=CARTESIAN_POINT('Origin',(-0.01550000000001,0.,-0.01550000000001));
#31456=CARTESIAN_POINT('',(0.0142705,0.,-0.0155));
#31457=CARTESIAN_POINT('Origin',(0.01550000000001,0.,-0.01550000000001));
#31458=CARTESIAN_POINT('',(-0.0167295,0.,0.0155));
#31459=CARTESIAN_POINT('Origin',(-0.01550000000001,0.,0.01550000000001));
#31460=CARTESIAN_POINT('',(-0.0109,0.,1.33486501107061E-18));
#31461=CARTESIAN_POINT('Origin',(0.,0.,0.));
#31462=CARTESIAN_POINT('Origin',(0.019,-0.0025,0.00403858223313768));
#31463=CARTESIAN_POINT('',(0.0185,-0.002,0.00766295090390226));
#31464=CARTESIAN_POINT('',(0.0185,-0.002,-0.00766295090390227));
#31465=CARTESIAN_POINT('',(0.01850000000001,-0.00200000000001,0.00403858223314768));
#31466=CARTESIAN_POINT('',(0.0195,-0.003,-0.00807716446627536));
#31467=CARTESIAN_POINT('',(0.01850000000001,-0.00200000000001,-0.00766295090391227));
#31468=CARTESIAN_POINT('',(0.0195,-0.003,0.00807716446627536));
#31469=CARTESIAN_POINT('',(0.01950000000001,-0.00300000000001,0.00403858223314768));
#31470=CARTESIAN_POINT('',(0.01850000000001,-0.00200000000001,0.00766295090391226));
#31471=CARTESIAN_POINT('Origin',(0.0162907377259756,-0.0025,-0.0105793199591133));
#31472=CARTESIAN_POINT('',(0.00766295090390227,-0.002,-0.0185));
#31473=CARTESIAN_POINT('',(0.0159371843353923,-0.00200000000001,-0.01022576656853));
#31474=CARTESIAN_POINT('',(0.00807716446627536,-0.003,-0.0195));
#31475=CARTESIAN_POINT('',(0.00766295090391227,-0.00200000000001,-0.01850000000001));
#31476=CARTESIAN_POINT('',(0.0166442911165789,-0.00300000000001,-0.0109328733497165));
#31477=CARTESIAN_POINT('Origin',(0.00403858223313768,-0.0025,-0.019));
#31478=CARTESIAN_POINT('',(-0.00766295090390227,-0.002,-0.0185));
#31479=CARTESIAN_POINT('',(0.00403858223314768,-0.00200000000001,-0.01850000000001));
#31480=CARTESIAN_POINT('',(-0.00807716446627536,-0.003,-0.0195));
#31481=CARTESIAN_POINT('',(-0.00766295090391227,-0.00200000000001,-0.01850000000001));
#31482=CARTESIAN_POINT('',(0.00403858223314768,-0.00300000000001,-0.01950000000001));
#31483=CARTESIAN_POINT('Origin',(-0.0105793199591133,-0.0025,-0.0162907377259756));
#31484=CARTESIAN_POINT('',(-0.0195,-0.003,-0.00807716446627536));
#31485=CARTESIAN_POINT('',(-0.0109328733497165,-0.00300000000001,-0.0166442911165788));
#31486=CARTESIAN_POINT('',(-0.0185,-0.002,-0.00766295090390226));
#31487=CARTESIAN_POINT('',(-0.01022576656853,-0.00200000000001,-0.0159371843353923));
#31488=CARTESIAN_POINT('',(-0.01850000000001,-0.00200000000001,-0.00766295090391226));
#31489=CARTESIAN_POINT('Origin',(-0.019,-0.0025,-0.00403858223313768));
#31490=CARTESIAN_POINT('',(-0.0195,-0.003,0.00807716446627536));
#31491=CARTESIAN_POINT('',(-0.01950000000001,-0.00300000000001,-0.00403858223314768));
#31492=CARTESIAN_POINT('',(-0.0185,-0.002,0.00766295090390227));
#31493=CARTESIAN_POINT('',(-0.01850000000001,-0.00200000000001,-0.00403858223314768));
#31494=CARTESIAN_POINT('',(-0.01850000000001,-0.00200000000001,0.00766295090391227));
#31495=CARTESIAN_POINT('Origin',(-0.0162907377259756,-0.0025,0.0105793199591132));
#31496=CARTESIAN_POINT('',(-0.00807716446627536,-0.003,0.0195));
#31497=CARTESIAN_POINT('',(-0.0166442911165789,-0.00300000000001,0.0109328733497165));
#31498=CARTESIAN_POINT('',(-0.00766295090390226,-0.002,0.0185));
#31499=CARTESIAN_POINT('',(-0.0159371843353923,-0.00200000000001,0.01022576656853));
#31500=CARTESIAN_POINT('',(-0.00766295090391226,-0.00200000000001,0.01850000000001));
#31501=CARTESIAN_POINT('Origin',(-0.00403858223313768,-0.0025,0.019));
#31502=CARTESIAN_POINT('',(0.00807716446627536,-0.003,0.0195));
#31503=CARTESIAN_POINT('',(-0.00403858223314768,-0.00300000000001,0.01950000000001));
#31504=CARTESIAN_POINT('',(0.00766295090390227,-0.002,0.0185));
#31505=CARTESIAN_POINT('',(-0.00403858223314768,-0.00200000000001,0.01850000000001));
#31506=CARTESIAN_POINT('',(0.00766295090391227,-0.00200000000001,0.01850000000001));
#31507=CARTESIAN_POINT('Origin',(0.0105793199591133,-0.0025,0.0162907377259756));
#31508=CARTESIAN_POINT('',(0.0109328733497165,-0.00300000000001,0.0166442911165789));
#31509=CARTESIAN_POINT('',(0.01022576656853,-0.00200000000001,0.0159371843353923));
#31510=CARTESIAN_POINT('Origin',(-0.0195,-0.008,0.00807716446627536));
#31511=CARTESIAN_POINT('',(-0.00807716446628536,-0.00800000000001,0.01950000000001));
#31512=CARTESIAN_POINT('',(-0.01950000000001,-0.00800000000001,0.00807716446628536));
#31513=CARTESIAN_POINT('Origin',(-0.00807716446627536,-0.008,0.0195));
#31514=CARTESIAN_POINT('',(0.00807716446628536,-0.00800000000001,0.01950000000001));
#31515=CARTESIAN_POINT('Origin',(0.00807716446627536,-0.008,0.0195));
#31516=CARTESIAN_POINT('',(0.01950000000001,-0.00800000000001,0.00807716446628536));
#31517=CARTESIAN_POINT('Origin',(0.0195,-0.008,0.00807716446627536));
#31518=CARTESIAN_POINT('',(0.01950000000001,-0.00800000000001,-0.00807716446628536));
#31519=CARTESIAN_POINT('Origin',(3.33066907387547E-18,-0.002,-1.11022302462516E-18));
#31520=CARTESIAN_POINT('',(0.013,-0.00200000000001,-1.59204083889156E-18));
#31521=CARTESIAN_POINT('Origin',(0.,-0.00200000000001,0.));
#31522=CARTESIAN_POINT('Origin',(0.0208771815508047,-0.000124980961894549,
0.008));
#31523=CARTESIAN_POINT('',(0.0210043631016193,-0.000249961923799098,0.00800000000001));
#31524=CARTESIAN_POINT('Origin',(0.,0.001875,0.));
#31525=CARTESIAN_POINT('',(-0.01090000000001,0.00175000000001,0.));
#31526=CARTESIAN_POINT('',(0.0109,0.00175,1.33486501107062E-18));
#31527=CARTESIAN_POINT('Origin',(0.,0.00175000000001,0.));
#31528=CARTESIAN_POINT('',(0.01065,0.002,1.30424884109193E-18));
#31529=CARTESIAN_POINT('',(0.010775,0.001875,1.31955692608127E-18));
#31530=CARTESIAN_POINT('Origin',(0.,0.00200000000001,0.));
#31531=CARTESIAN_POINT('Origin',(0.,0.00175000000001,0.));
#31532=CARTESIAN_POINT('Origin',(0.,0.002,0.));
#31533=CARTESIAN_POINT('',(0.00475000000001,0.00200000000001,-5.81707229596217E-19));
#31534=CARTESIAN_POINT('Origin',(0.,0.00200000000001,0.));
#31535=CARTESIAN_POINT('Origin',(0.,0.,0.));
#31536=CARTESIAN_POINT('',(-0.0109,0.,1.33486501107061E-18));
#31537=CARTESIAN_POINT('Origin',(0.,0.001875,0.));
#31538=CARTESIAN_POINT('',(-0.00450000000001,0.00175000000001,0.));
#31539=CARTESIAN_POINT('',(0.00450000000001,0.00175000000001,-5.51091059617534E-19));
#31540=CARTESIAN_POINT('Origin',(0.,0.00175000000001,0.));
#31541=CARTESIAN_POINT('',(0.004625,0.001875,-5.66399144605651E-19));
#31542=CARTESIAN_POINT('Origin',(0.,0.00175000000001,0.));
#31543=CARTESIAN_POINT('Origin',(0.,-0.0587953551706409,0.));
#31544=CARTESIAN_POINT('',(-0.0045,0.000250000000010004,5.51091059616309E-19));
#31545=CARTESIAN_POINT('Origin',(0.,0.000250000000010004,0.));
#31546=CARTESIAN_POINT('',(-0.0045,-0.0587953551706409,5.51091059616309E-19));
#31547=CARTESIAN_POINT('Origin',(0.,0.000125000000000002,0.));
#31548=CARTESIAN_POINT('',(-0.00475,5.72458747072346E-19,-5.81707229594993E-19));
#31549=CARTESIAN_POINT('',(-0.004625,0.000125000000000002,-5.66399144605651E-19));
#31550=CARTESIAN_POINT('Origin',(0.,1.00005551115123E-14,0.));
#31551=CARTESIAN_POINT('Origin',(0.,5.55111512312578E-19,0.));
#31552=CARTESIAN_POINT('',(-0.006,1.00006114500673E-14,7.34788079488412E-19));
#31553=CARTESIAN_POINT('Origin',(0.,1.00005551115123E-14,0.));
#31554=CARTESIAN_POINT('Origin',(0.,-0.008875,0.));
#31555=CARTESIAN_POINT('',(0.013,-0.00875,-1.59204083889156E-18));
#31556=CARTESIAN_POINT('Origin',(0.,-0.00875000000001,0.));
#31557=CARTESIAN_POINT('',(0.01275,-0.009,-1.56142466891288E-18));
#31558=CARTESIAN_POINT('',(0.012875,-0.008875,-1.57673275390222E-18));
#31559=CARTESIAN_POINT('Origin',(0.,-0.00900000000001,0.));
#31560=CARTESIAN_POINT('Origin',(0.,-0.009,0.));
#31561=CARTESIAN_POINT('',(0.00825000000000294,-0.00900000000001176,1.01033360929693E-18));
#31562=CARTESIAN_POINT('Origin',(0.,-0.00900000000001,0.));
#31563=CARTESIAN_POINT('Origin',(0.,-0.008,0.));
#31564=CARTESIAN_POINT('',(0.013,-0.008,-1.59204083889156E-18));
#31565=CARTESIAN_POINT('Origin',(0.,-0.0085,0.));
#31566=CARTESIAN_POINT('',(-0.00800000000001,-0.00800000000001,0.));
#31567=CARTESIAN_POINT('',(0.00800000000000294,-0.00800000000001177,9.79717439318243E-19));
#31568=CARTESIAN_POINT('Origin',(0.,-0.00800000000001,0.));
#31569=CARTESIAN_POINT('',(0.008125,-0.0085,9.95025524307224E-19));
#31570=CARTESIAN_POINT('Origin',(0.,-0.00800000000001,0.));
#31571=CARTESIAN_POINT('Origin',(0.,-0.009,0.));
#31572=CARTESIAN_POINT('',(-0.008,-0.000750000000010002,9.79717439317883E-19));
#31573=CARTESIAN_POINT('',(-0.008,-0.009,9.79717439317883E-19));
#31574=CARTESIAN_POINT('Origin',(0.,-0.00075000000001,0.));
#31575=CARTESIAN_POINT('Origin',(0.0155,-0.0607953551706409,0.0155));
#31576=CARTESIAN_POINT('',(0.0142705,-0.0607953551706409,0.0155));
#31577=CARTESIAN_POINT('Origin',(-0.0155,-0.0607953551706409,-0.0155));
#31578=CARTESIAN_POINT('',(-0.0167295,-0.0607953551706409,-0.0155));
#31579=CARTESIAN_POINT('Origin',(0.0155,-0.0607953551706409,-0.0155));
#31580=CARTESIAN_POINT('',(0.0142705,-0.0607953551706409,-0.0155));
#31581=CARTESIAN_POINT('Origin',(-0.0155,-0.0607953551706409,0.0155));
#31582=CARTESIAN_POINT('',(-0.0167295,-0.0607953551706409,0.0155));
#31583=CARTESIAN_POINT('Origin',(0.,-0.00075,0.));
#31584=CARTESIAN_POINT('',(-0.006,-0.00075000000001,7.34788079488412E-19));
#31585=CARTESIAN_POINT('Origin',(0.,-0.00075000000001,0.));
#31586=CARTESIAN_POINT('',(-0.006,-0.00075,7.34788079488412E-19));
#31587=CARTESIAN_POINT('Origin',(0.,-0.00075,0.));
#31588=CARTESIAN_POINT('Origin',(-0.0195,-0.008,-0.00807716446627536));
#31589=CARTESIAN_POINT('',(-0.01950000000001,-0.00800000000001,-0.00807716446628536));
#31590=CARTESIAN_POINT('Origin',(-0.00807716446627536,-0.008,-0.0195));
#31591=CARTESIAN_POINT('',(-0.00807716446628536,-0.00800000000001,-0.01950000000001));
#31592=CARTESIAN_POINT('Origin',(0.00807716446627536,-0.008,-0.0195));
#31593=CARTESIAN_POINT('',(0.00807716446628536,-0.00800000000001,-0.01950000000001));
#31594=CARTESIAN_POINT('Origin',(0.0195,-0.008,-0.00807716446627536));
#31595=CARTESIAN_POINT('Origin',(0.021,0.,0.016));
#31596=CARTESIAN_POINT('',(0.,0.,0.));
#31597=CARTESIAN_POINT('Origin',(-0.0126992616256242,-0.008,-0.00360121565085291));
#31598=CARTESIAN_POINT('',(-0.0126265137841014,-0.008,-0.00384039707060321));
#31599=CARTESIAN_POINT('',(-0.0129397779442914,-0.008,-0.00366942049272513));
#31600=CARTESIAN_POINT('Origin',(-0.0126992616256342,-0.00799999999999,
-0.00360121565086291));
#31601=CARTESIAN_POINT('',(-0.0129397779442914,-0.024,-0.00366942049272513));
#31602=CARTESIAN_POINT('',(-0.0129397779443014,-0.00799999999999,-0.00366942049273513));
#31603=CARTESIAN_POINT('',(-0.0126265137841014,-0.024,-0.00384039707060321));
#31604=CARTESIAN_POINT('Origin',(-0.0126992616256342,-0.02400000000001,
-0.00360121565086291));
#31605=CARTESIAN_POINT('',(-0.0126265137841114,-0.00799999999999,-0.00384039707061321));
#31606=CARTESIAN_POINT('Origin',(-4.44089209850063E-17,-0.008,6.72997231505748E-33));
#31607=CARTESIAN_POINT('',(-0.0130408866654485,-0.008,-0.0032920776082785));
#31608=CARTESIAN_POINT('Origin',(-4.44089209850063E-17,-0.00799999999999,
6.72997231505748E-33));
#31609=CARTESIAN_POINT('',(-0.0130408866654485,-0.024,-0.0032920776082785));
#31610=CARTESIAN_POINT('',(-0.0130408866654585,-0.00799999999999,-0.0032920776082885));
#31611=CARTESIAN_POINT('Origin',(-4.44089209850063E-17,-0.02400000000001,
6.72997231505748E-33));
#31612=CARTESIAN_POINT('Origin',(-0.0127984910025219,-0.008,-0.00323088657466738));
#31613=CARTESIAN_POINT('',(-0.0128550802335678,-0.008,-0.00298737546828897));
#31614=CARTESIAN_POINT('Origin',(-0.0127984910025319,-0.00799999999999,
-0.00323088657467738));
#31615=CARTESIAN_POINT('',(-0.0128550802335678,-0.024,-0.00298737546828897));
#31616=CARTESIAN_POINT('',(-0.0128550802335778,-0.00799999999999,-0.00298737546829897));
#31617=CARTESIAN_POINT('Origin',(-0.0127984910025319,-0.02400000000001,
-0.00323088657467738));
#31618=CARTESIAN_POINT('Origin',(-0.0126625775316771,-0.008,-0.00294264001438602));
#31619=CARTESIAN_POINT('',(-0.0126625775316771,-0.008,-0.00294264001438602));
#31620=CARTESIAN_POINT('',(-0.0125348531511851,-0.00799999999999,-0.00291295831081412));
#31621=CARTESIAN_POINT('',(-0.0126625775316771,-0.024,-0.00294264001438602));
#31622=CARTESIAN_POINT('',(-0.0126625775316871,-0.016,-0.00294264001439602));
#31623=CARTESIAN_POINT('',(-0.0125348531511851,-0.02400000000001,-0.00291295831081412));
#31624=CARTESIAN_POINT('Origin',(-0.0130606706482359,-0.008,-0.00191282048773811));
#31625=CARTESIAN_POINT('',(-0.0130197646145518,-0.008,-0.00215945117603184));
#31626=CARTESIAN_POINT('',(-0.0133080318347555,-0.008,-0.00194904814849073));
#31627=CARTESIAN_POINT('Origin',(-0.0130606706482459,-0.00799999999999,
-0.00191282048774811));
#31628=CARTESIAN_POINT('',(-0.0133080318347555,-0.024,-0.00194904814849073));
#31629=CARTESIAN_POINT('',(-0.0133080318347655,-0.00799999999999,-0.00194904814850073));
#31630=CARTESIAN_POINT('',(-0.0130197646145518,-0.024,-0.00215945117603184));
#31631=CARTESIAN_POINT('Origin',(-0.0130606706482459,-0.02400000000001,
-0.00191282048774811));
#31632=CARTESIAN_POINT('',(-0.0130197646145618,-0.00799999999999,-0.00215945117604184));
#31633=CARTESIAN_POINT('Origin',(-4.44089209850063E-17,-0.008,6.72997231505748E-33));
#31634=CARTESIAN_POINT('',(-0.0133590224269186,-0.008,-0.00156173614835727));
#31635=CARTESIAN_POINT('Origin',(-4.44089209850063E-17,-0.00799999999999,
6.72997231505748E-33));
#31636=CARTESIAN_POINT('',(-0.0133590224269186,-0.024,-0.00156173614835727));
#31637=CARTESIAN_POINT('',(-0.0133590224269286,-0.00799999999999,-0.00156173614836727));
#31638=CARTESIAN_POINT('Origin',(-4.44089209850063E-17,-0.02400000000001,
6.72997231505748E-33));
#31639=CARTESIAN_POINT('Origin',(-0.0131107134598755,-0.008,-0.00153270759541383));
#31640=CARTESIAN_POINT('',(-0.0131350339847262,-0.008,-0.00128389338345842));
#31641=CARTESIAN_POINT('Origin',(-0.0131107134598855,-0.00799999999999,
-0.00153270759542383));
#31642=CARTESIAN_POINT('',(-0.0131350339847262,-0.024,-0.00128389338345842));
#31643=CARTESIAN_POINT('',(-0.0131350339847362,-0.00799999999999,-0.00128389338346842));
#31644=CARTESIAN_POINT('Origin',(-0.0131107134598855,-0.02400000000001,
-0.00153270759542383));
#31645=CARTESIAN_POINT('Origin',(-0.0129383390216809,-0.008,-0.00126466729223498));
#31646=CARTESIAN_POINT('',(-0.0129383390216809,-0.008,-0.00126466729223498));
#31647=CARTESIAN_POINT('',(-0.0129458744527519,-0.00799999999999,-0.00126540384839641));
#31648=CARTESIAN_POINT('',(-0.0129383390216809,-0.024,-0.00126466729223498));
#31649=CARTESIAN_POINT('',(-0.0129383390216909,-0.016,-0.00126466729224498));
#31650=CARTESIAN_POINT('',(-0.0129458744527519,-0.02400000000001,-0.00126540384839641));
#31651=CARTESIAN_POINT('Origin',(-0.0131986079749541,-0.008,-0.000191696435744077));
#31652=CARTESIAN_POINT('',(-0.0131902436626865,-0.008,-0.000441556473125586));
#31653=CARTESIAN_POINT('',(-0.0134485816108434,-0.008,-0.000195327050057411));
#31654=CARTESIAN_POINT('Origin',(-0.0131986079749641,-0.00799999999999,
-0.000191696435754077));
#31655=CARTESIAN_POINT('',(-0.0134485816108434,-0.024,-0.000195327050057411));
#31656=CARTESIAN_POINT('',(-0.0134485816108534,-0.00799999999999,-0.000195327050067411));
#31657=CARTESIAN_POINT('',(-0.0131902436626865,-0.024,-0.000441556473125586));
#31658=CARTESIAN_POINT('Origin',(-0.0131986079749641,-0.02400000000001,
-0.000191696435754077));
#31659=CARTESIAN_POINT('',(-0.0131902436626965,-0.00799999999999,-0.000441556473135586));
#31660=CARTESIAN_POINT('Origin',(-4.44089209850063E-17,-0.008,6.72997231505748E-33));
#31661=CARTESIAN_POINT('',(-0.0134485816108434,-0.008,0.000195327050057416));
#31662=CARTESIAN_POINT('Origin',(-4.44089209850063E-17,-0.00799999999999,
6.72997231505748E-33));
#31663=CARTESIAN_POINT('',(-0.0134485816108434,-0.024,0.000195327050057416));
#31664=CARTESIAN_POINT('',(-0.0134485816108534,-0.00799999999999,0.000195327050067416));
#31665=CARTESIAN_POINT('Origin',(-4.44089209850063E-17,-0.02400000000001,
6.72997231505748E-33));
#31666=CARTESIAN_POINT('Origin',(-0.0131986079749541,-0.008,0.000191696435744081));
#31667=CARTESIAN_POINT('',(-0.0131902436626865,-0.008,0.00044155647312559));
#31668=CARTESIAN_POINT('Origin',(-0.0131986079749641,-0.00799999999999,
0.000191696435754081));
#31669=CARTESIAN_POINT('',(-0.0131902436626865,-0.024,0.00044155647312559));
#31670=CARTESIAN_POINT('',(-0.0131902436626965,-0.00799999999999,0.00044155647313559));
#31671=CARTESIAN_POINT('Origin',(-0.0131986079749641,-0.02400000000001,
0.000191696435754081));
#31672=CARTESIAN_POINT('Origin',(-0.0129927219438385,-0.008,0.000434944237918218));
#31673=CARTESIAN_POINT('',(-0.0129927219438385,-0.008,0.000434944237918218));
#31674=CARTESIAN_POINT('',(-0.0130276266077339,-0.00799999999999,0.000436112706129036));
#31675=CARTESIAN_POINT('',(-0.0129927219438385,-0.024,0.000434944237918218));
#31676=CARTESIAN_POINT('',(-0.0129927219438485,-0.016,0.000434944237928218));
#31677=CARTESIAN_POINT('',(-0.0130276266077339,-0.02400000000001,0.000436112706129036));
#31678=CARTESIAN_POINT('Origin',(-0.0131107134598755,-0.008,0.00153270759541383));
#31679=CARTESIAN_POINT('',(-0.0131350339847262,-0.008,0.00128389338345843));
#31680=CARTESIAN_POINT('',(-0.0133590224269186,-0.008,0.00156173614835727));
#31681=CARTESIAN_POINT('Origin',(-0.0131107134598855,-0.00799999999999,
0.00153270759542383));
#31682=CARTESIAN_POINT('',(-0.0133590224269186,-0.024,0.00156173614835727));
#31683=CARTESIAN_POINT('',(-0.0133590224269286,-0.00799999999999,0.00156173614836727));
#31684=CARTESIAN_POINT('',(-0.0131350339847262,-0.024,0.00128389338345843));
#31685=CARTESIAN_POINT('Origin',(-0.0131107134598855,-0.02400000000001,
0.00153270759542383));
#31686=CARTESIAN_POINT('',(-0.0131350339847362,-0.00799999999999,0.00128389338346843));
#31687=CARTESIAN_POINT('Origin',(-4.44089209850063E-17,-0.008,6.72997231505748E-33));
#31688=CARTESIAN_POINT('',(-0.0133080318347555,-0.008,0.00194904814849073));
#31689=CARTESIAN_POINT('Origin',(-4.44089209850063E-17,-0.00799999999999,
6.72997231505748E-33));
#31690=CARTESIAN_POINT('',(-0.0133080318347555,-0.024,0.00194904814849073));
#31691=CARTESIAN_POINT('',(-0.0133080318347655,-0.00799999999999,0.00194904814850073));
#31692=CARTESIAN_POINT('Origin',(-4.44089209850063E-17,-0.02400000000001,
6.72997231505748E-33));
#31693=CARTESIAN_POINT('Origin',(-0.0130606706482359,-0.008,0.00191282048773811));
#31694=CARTESIAN_POINT('',(-0.0130197646145518,-0.008,0.00215945117603184));
#31695=CARTESIAN_POINT('Origin',(-0.0130606706482459,-0.00799999999999,
0.00191282048774811));
#31696=CARTESIAN_POINT('',(-0.0130197646145518,-0.024,0.00215945117603184));
#31697=CARTESIAN_POINT('',(-0.0130197646145618,-0.00799999999999,0.00215945117604184));
#31698=CARTESIAN_POINT('Origin',(-0.0130606706482459,-0.02400000000001,
0.00191282048774811));
#31699=CARTESIAN_POINT('Origin',(-0.0128247957912739,-0.008,0.00212711375157131));
#31700=CARTESIAN_POINT('',(-0.0128247957912739,-0.008,0.00212711375157131));
#31701=CARTESIAN_POINT('',(-0.0127759261415696,-0.00799999999999,0.00211900825769013));
#31702=CARTESIAN_POINT('',(-0.0128247957912739,-0.024,0.00212711375157131));
#31703=CARTESIAN_POINT('',(-0.0128247957912839,-0.016,0.00212711375158131));
#31704=CARTESIAN_POINT('',(-0.0127759261415696,-0.02400000000001,0.00211900825769013));
#31705=CARTESIAN_POINT('Origin',(-0.0127984910025219,-0.008,0.00323088657466738));
#31706=CARTESIAN_POINT('',(-0.0128550802335678,-0.008,0.00298737546828897));
#31707=CARTESIAN_POINT('',(-0.0130408866654485,-0.008,0.0032920776082785));
#31708=CARTESIAN_POINT('Origin',(-0.0127984910025319,-0.00799999999999,
0.00323088657467738));
#31709=CARTESIAN_POINT('',(-0.0130408866654485,-0.024,0.0032920776082785));
#31710=CARTESIAN_POINT('',(-0.0130408866654585,-0.00799999999999,0.0032920776082885));
#31711=CARTESIAN_POINT('',(-0.0128550802335678,-0.024,0.00298737546828897));
#31712=CARTESIAN_POINT('Origin',(-0.0127984910025319,-0.02400000000001,
0.00323088657467738));
#31713=CARTESIAN_POINT('',(-0.0128550802335778,-0.00799999999999,0.00298737546829897));
#31714=CARTESIAN_POINT('Origin',(-4.44089209850063E-17,-0.008,6.72997231505748E-33));
#31715=CARTESIAN_POINT('',(-0.0129397779442914,-0.008,0.00366942049272513));
#31716=CARTESIAN_POINT('Origin',(-4.44089209850063E-17,-0.00799999999999,
6.72997231505748E-33));
#31717=CARTESIAN_POINT('',(-0.0129397779442914,-0.024,0.00366942049272513));
#31718=CARTESIAN_POINT('',(-0.0129397779443014,-0.00799999999999,0.00366942049273513));
#31719=CARTESIAN_POINT('Origin',(-4.44089209850063E-17,-0.02400000000001,
6.72997231505748E-33));
#31720=CARTESIAN_POINT('Origin',(-0.0126992616256242,-0.008,0.00360121565085292));
#31721=CARTESIAN_POINT('',(-0.0126265137841014,-0.008,0.00384039707060321));
#31722=CARTESIAN_POINT('Origin',(-0.0126992616256342,-0.00799999999999,
0.00360121565086292));
#31723=CARTESIAN_POINT('',(-0.0126265137841014,-0.024,0.00384039707060321));
#31724=CARTESIAN_POINT('',(-0.0126265137841114,-0.00799999999999,0.00384039707061321));
#31725=CARTESIAN_POINT('Origin',(-0.0126992616256342,-0.02400000000001,
0.00360121565086292));
#31726=CARTESIAN_POINT('Origin',(-0.0124374338270155,-0.008,0.00378288775918766));
#31727=CARTESIAN_POINT('',(-0.0124374338270155,-0.008,0.00378288775918766));
#31728=CARTESIAN_POINT('',(-0.0122036407116943,-0.00799999999999,0.00371177878877263));
#31729=CARTESIAN_POINT('',(-0.0124374338270155,-0.024,0.00378288775918766));
#31730=CARTESIAN_POINT('',(-0.0124374338270255,-0.016,0.00378288775919766));
#31731=CARTESIAN_POINT('',(-0.0122036407116943,-0.02400000000001,0.00371177878877263));
#31732=CARTESIAN_POINT('Origin',(-0.0131008975231583,-0.008,0.00304450063026861));
#31733=CARTESIAN_POINT('',(-0.0126625775316771,-0.024,0.00294264001438602));
#31734=CARTESIAN_POINT('',(-0.0127540131469256,-0.02400000000001,0.00296388861875542));
#31735=CARTESIAN_POINT('',(-0.0126625775316771,-0.008,0.00294264001438602));
#31736=CARTESIAN_POINT('',(-0.0126625775316871,-0.016,0.00294264001439602));
#31737=CARTESIAN_POINT('',(-0.0127540131469256,-0.00799999999999,0.00296388861875542));
#31738=CARTESIAN_POINT('Origin',(-0.0133862046032006,-0.008,0.00130844423696619));
#31739=CARTESIAN_POINT('',(-0.0129383390216809,-0.024,0.00126466729223498));
#31740=CARTESIAN_POINT('',(-0.0131698072435117,-0.02400000000001,0.00128729232076202));
#31741=CARTESIAN_POINT('',(-0.0129383390216809,-0.008,0.00126466729223498));
#31742=CARTESIAN_POINT('',(-0.0129383390216909,-0.016,0.00126466729224498));
#31743=CARTESIAN_POINT('',(-0.0131698072435117,-0.00799999999999,0.00128729232076202));
#31744=CARTESIAN_POINT('Origin',(-0.0132687310302026,-0.008,-0.00220074461220262));
#31745=CARTESIAN_POINT('',(-0.0128247957912739,-0.024,-0.0021271137515713));
#31746=CARTESIAN_POINT('',(-0.0129978937610339,-0.02400000000001,-0.00215582368800578));
#31747=CARTESIAN_POINT('',(-0.0128247957912739,-0.008,-0.0021271137515713));
#31748=CARTESIAN_POINT('',(-0.0128247957912839,-0.016,-0.0021271137515813));
#31749=CARTESIAN_POINT('',(-0.0129978937610339,-0.00799999999999,-0.00215582368800578));
#31750=CARTESIAN_POINT('Origin',(-0.012867960382566,-0.008,-0.00391383387392877));
#31751=CARTESIAN_POINT('',(-0.0124374338270155,-0.024,-0.00378288775918766));
#31752=CARTESIAN_POINT('',(-0.0124189039894696,-0.02400000000001,-0.00377725184614318));
#31753=CARTESIAN_POINT('',(-0.0124374338270155,-0.008,-0.00378288775918766));
#31754=CARTESIAN_POINT('',(-0.0124374338270255,-0.016,-0.00378288775919766));
#31755=CARTESIAN_POINT('',(-0.0124189039894696,-0.00799999999999,-0.00377725184614318));
#31756=CARTESIAN_POINT('Origin',(-4.44089209850063E-17,-0.016,6.72997231505748E-33));
#31757=CARTESIAN_POINT('',(-0.0122543393841983,-0.008,0.00433948917003902));
#31758=CARTESIAN_POINT('Origin',(-4.44089209850063E-17,-0.00799999999999,
6.72997231505748E-33));
#31759=CARTESIAN_POINT('',(-0.0122543393841983,-0.024,0.00433948917003902));
#31760=CARTESIAN_POINT('',(-0.0122543393842083,-0.016,0.00433948917004902));
#31761=CARTESIAN_POINT('Origin',(-4.44089209850063E-17,-0.02400000000001,
6.72997231505748E-33));
#31762=CARTESIAN_POINT('Origin',(-4.44089209850063E-17,-0.016,6.72997231505748E-33));
#31763=CARTESIAN_POINT('Origin',(-4.44089209850063E-17,-0.02400000000001,
6.72997231505748E-33));
#31764=CARTESIAN_POINT('Origin',(-4.44089209850063E-17,-0.00799999999999,
6.72997231505748E-33));
#31765=CARTESIAN_POINT('Origin',(-0.0130771696920992,-0.024,1.11022302462517E-18));
#31766=CARTESIAN_POINT('',(-0.0131027167261813,-0.024,0.00463991534334942));
#31767=CARTESIAN_POINT('',(-0.0131027167261913,-0.02400000000001,0.00463991534335942));
#31768=CARTESIAN_POINT('',(-0.0131027167261813,-0.024,-0.00463991534334942));
#31769=CARTESIAN_POINT('Origin',(-4.44089209850063E-17,-0.02400000000001,
6.72997231505748E-33));
#31770=CARTESIAN_POINT('',(-0.0122543393841983,-0.024,-0.00433948917003902));
#31771=CARTESIAN_POINT('',(-0.0122543393842083,-0.02400000000001,-0.00433948917004902));
#31772=CARTESIAN_POINT('Origin',(-4.44089209850063E-17,-0.02400000000001,
6.72997231505748E-33));
#31773=CARTESIAN_POINT('Origin',(-4.44089209850063E-17,-0.02400000000001,
6.72997231505748E-33));
#31774=CARTESIAN_POINT('',(-0.0129927219438385,-0.024,-0.000434944237918213));
#31775=CARTESIAN_POINT('Origin',(-4.44089209850063E-17,-0.02400000000001,
6.72997231505748E-33));
#31776=CARTESIAN_POINT('',(-0.0132525006413773,-0.02400000000001,-0.000443640587169925));
#31777=CARTESIAN_POINT('Origin',(-4.44089209850063E-17,-0.02400000000001,
6.72997231505748E-33));
#31778=CARTESIAN_POINT('Origin',(-4.44089209850063E-17,-0.016,6.72997231505748E-33));
#31779=CARTESIAN_POINT('',(-0.0129927219438385,-0.008,-0.000434944237918213));
#31780=CARTESIAN_POINT('Origin',(-4.44089209850063E-17,-0.00799999999999,
6.72997231505748E-33));
#31781=CARTESIAN_POINT('',(-0.0129927219438485,-0.016,-0.000434944237928214));
#31782=CARTESIAN_POINT('Origin',(-4.44089209850063E-17,-0.016,6.72997231505748E-33));
#31783=CARTESIAN_POINT('',(-0.0122543393841983,-0.008,-0.00433948917003902));
#31784=CARTESIAN_POINT('',(-0.0122543393842083,-0.016,-0.00433948917004902));
#31785=CARTESIAN_POINT('Origin',(-4.44089209850063E-17,-0.00799999999999,
6.72997231505748E-33));
#31786=CARTESIAN_POINT('Origin',(-0.0134424700111252,-0.008,-0.00045));
#31787=CARTESIAN_POINT('',(-0.0132525006413773,-0.00799999999999,-0.000443640587169925));
#31788=CARTESIAN_POINT('Origin',(-4.44089209850063E-17,-0.016,6.72997231505748E-33));
#31789=CARTESIAN_POINT('Origin',(-4.44089209850063E-17,-0.00799999999999,
6.72997231505748E-33));
#31790=CARTESIAN_POINT('Origin',(-0.0131027167261813,-0.016,0.00463991534334942));
#31791=CARTESIAN_POINT('',(-0.0131027167261813,-0.008,0.00463991534334942));
#31792=CARTESIAN_POINT('',(-0.0131027167261913,-0.00799999999999,0.00463991534335942));
#31793=CARTESIAN_POINT('',(-0.0131027167261913,-0.016,0.00463991534335942));
#31794=CARTESIAN_POINT('Origin',(-4.44089209850063E-17,-0.016,6.72997231505748E-33));
#31795=CARTESIAN_POINT('',(-0.0131027167261813,-0.008,-0.00463991534334942));
#31796=CARTESIAN_POINT('Origin',(-4.44089209850063E-17,-0.00799999999999,
6.72997231505748E-33));
#31797=CARTESIAN_POINT('',(-0.0131027167261913,-0.016,-0.00463991534335942));
#31798=CARTESIAN_POINT('Origin',(-0.0122543393841983,-0.016,-0.00433948917003902));
#31799=CARTESIAN_POINT('',(-0.0122543393842083,-0.00799999999999,-0.00433948917004902));
#31800=CARTESIAN_POINT('Origin',(-4.44089209850063E-17,-0.016,6.72997231505748E-33));
#31801=CARTESIAN_POINT('Origin',(-4.44089209850063E-17,-0.00799999999999,
6.72997231505748E-33));
#31802=CARTESIAN_POINT('Origin',(-0.0130771696920992,-0.008,1.11022302462517E-18));
#31803=CARTESIAN_POINT('',(0.,0.,0.));
#31804=CARTESIAN_POINT('Origin',(-4.68201057504096E-17,0.0215,5.80537005579265E-33));
#31805=CARTESIAN_POINT('',(0.000529682692573917,0.021249999999998,-0.00244324297711006));
#31806=CARTESIAN_POINT('',(0.000423746154058535,0.0217500000000012,-0.00195459438168533));
#31807=CARTESIAN_POINT('',(0.000476714423316139,0.0215,-0.00219891867939729));
#31808=CARTESIAN_POINT('',(-0.000529682692573586,0.02125000000001,0.0024432429771081));
#31809=CARTESIAN_POINT('Origin',(-4.68034607815872E-17,0.02125000000001,
5.84812570055634E-33));
#31810=CARTESIAN_POINT('',(0.00163678476614231,0.02125,0.00188969194032369));
#31811=CARTESIAN_POINT('Origin',(-4.68034607815872E-17,0.02125000000001,
5.84812570055634E-33));
#31812=CARTESIAN_POINT('',(0.00195459438168643,0.02175,0.000423746154058832));
#31813=CARTESIAN_POINT('Ctrl Pts',(0.00163678476614996,0.02125000000001,
0.00188969194033559));
#31814=CARTESIAN_POINT('Ctrl Pts',(0.00181334566367447,0.02175000000001,
0.0010752776146329));
#31815=CARTESIAN_POINT('Ctrl Pts',(0.00195459438169832,0.02175000000001,
0.000423746154051177));
#31816=CARTESIAN_POINT('Origin',(-4.68367507192334E-17,0.02175000000001,
5.76261441102555E-33));
#31817=CARTESIAN_POINT('Origin',(-4.68201057504096E-17,0.0215,5.80537005579265E-33));
#31818=CARTESIAN_POINT('Origin',(-4.68367507192334E-17,0.02175000000001,
5.76261441102555E-33));
#31819=CARTESIAN_POINT('',(0.00227240399723056,0.02125,-0.00104219963220603));
#31820=CARTESIAN_POINT('Ctrl Pts',(0.00195459438169832,0.02175000000001,
0.000423746154051177));
#31821=CARTESIAN_POINT('Ctrl Pts',(0.00209584309971794,0.02175000000001,
-0.000227785306511001));
#31822=CARTESIAN_POINT('Ctrl Pts',(0.00227240399724245,0.02125000000001,
-0.00104219963221369));
#31823=CARTESIAN_POINT('Origin',(-4.68034607815872E-17,0.02125000000001,
5.84812570055634E-33));
#31824=CARTESIAN_POINT('Origin',(-4.36409167051929E-17,-0.02625,1.39716982059834E-32));
#31825=CARTESIAN_POINT('',(-0.000423746154058875,-0.02550000000001,0.00195459438168648));
#31826=CARTESIAN_POINT('Origin',(-4.36908516116616E-17,-0.02550000000001,
1.38434312716889E-32));
#31827=CARTESIAN_POINT('',(-0.000423746154058875,-0.02625000000001,0.00195459438168648));
#31828=CARTESIAN_POINT('',(-0.000423746154058875,-0.02625,0.00195459438168648));
#31829=CARTESIAN_POINT('Origin',(-4.36409167051922E-17,-0.02625000000001,
1.39716982059851E-32));
#31830=CARTESIAN_POINT('Origin',(-4.36409167051929E-17,-0.02625,1.39716982059834E-32));
#31831=CARTESIAN_POINT('',(-0.000529682692573583,-0.02625000000001,0.0024432429771081));
#31832=CARTESIAN_POINT('Origin',(-4.36409167051922E-17,-0.02625000000001,
1.39716982059851E-32));
#31833=CARTESIAN_POINT('Origin',(-4.36908516116622E-17,-0.0255,1.38434312716872E-32));
#31834=CARTESIAN_POINT('',(-0.000529682692573583,-0.02550000000001,0.0024432429771081));
#31835=CARTESIAN_POINT('Origin',(-4.36908516116616E-17,-0.02550000000001,
1.38434312716889E-32));
#31836=CARTESIAN_POINT('Origin',(-4.50723840239816E-17,-0.00475,1.02947127561593E-32));
#31837=CARTESIAN_POINT('',(0.00163678476614231,0.00375,0.00188969194032369));
#31838=CARTESIAN_POINT('',(0.00163678476614996,-0.00475,0.00188969194033558));
#31839=CARTESIAN_POINT('',(-0.000529682692573585,-0.00475,0.0024432429771081));
#31840=CARTESIAN_POINT('',(0.00227240399723056,0.00375,-0.00104219963220603));
#31841=CARTESIAN_POINT('',(0.00227240399724245,-0.00475,-0.00104219963221368));
#31842=CARTESIAN_POINT('Origin',(-4.56383129639685E-17,0.00375000000001,
8.8410208341341E-33));
#31843=CARTESIAN_POINT('Origin',(0.00163678476614231,0.02175,0.00188969194032369));
#31844=CARTESIAN_POINT('',(0.00227240399724245,0.00375000000001,-0.00104219963221368));
#31845=CARTESIAN_POINT('Origin',(0.00219891867939725,0.00375,0.000476714423316185));
#31846=CARTESIAN_POINT('Origin',(-4.50723840239816E-17,-0.00475,1.02947127561593E-32));
#31847=CARTESIAN_POINT('',(-0.000529682692575702,-0.03075000000001,0.00244324297711787));
#31848=CARTESIAN_POINT('',(-0.000529682692573585,-0.00475,0.0024432429771081));
#31849=CARTESIAN_POINT('',(0.000529682692573497,-0.03075,-0.0024432429771081));
#31850=CARTESIAN_POINT('Origin',(-4.3341307266376E-17,-0.03075000000001,
1.47412998117623E-32));
#31851=CARTESIAN_POINT('Origin',(-4.3341307266376E-17,-0.03075000000001,
1.47412998117623E-32));
#31852=CARTESIAN_POINT('Origin',(-4.33246622975535E-17,-0.031,1.47840554565259E-32));
#31853=CARTESIAN_POINT('',(0.000423746154058788,-0.03125,-0.00195459438168648));
#31854=CARTESIAN_POINT('',(0.000476714423316142,-0.031,-0.00219891867939729));
#31855=CARTESIAN_POINT('Origin',(-4.33080173287297E-17,-0.03125000000001,
1.4826811101293E-32));
#31856=CARTESIAN_POINT('Origin',(-4.33080173287304E-17,-0.03125,1.48268111012913E-32));
#31857=CARTESIAN_POINT('Origin',(-4.68367507192327E-17,0.02175,5.76261441102726E-33));
#31858=CARTESIAN_POINT('',(0.,0.,0.));
#31859=CARTESIAN_POINT('Origin',(0.0211500000000181,-0.024,-0.00793218971944487));
#31860=CARTESIAN_POINT('',(0.0211500000000181,-0.03075,-0.00793218971944487));
#31861=CARTESIAN_POINT('',(0.0211500000000182,-0.03074999999999,-0.00800000000000999));
#31862=CARTESIAN_POINT('',(0.0211500000000189,-0.03075,-0.00884109485971803));
#31863=CARTESIAN_POINT('',(0.0211500000000181,-0.031,-0.00793218971944487));
#31864=CARTESIAN_POINT('',(0.0211500000000181,-0.024,-0.00793218971944487));
#31865=CARTESIAN_POINT('',(0.0211500000000182,-0.031,-0.00800000000000999));
#31866=CARTESIAN_POINT('',(0.0211500000000189,-0.031,-0.00884109485971803));
#31867=CARTESIAN_POINT('',(0.0211500000000182,-0.0275,-0.008));
#31868=CARTESIAN_POINT('Origin',(0.02115,-0.024,0.0129631448730622));
#31869=CARTESIAN_POINT('',(0.0211500000000044,-0.031,0.00793218971944469));
#31870=CARTESIAN_POINT('',(0.0211500000000043,-0.031,0.00800000000001137));
#31871=CARTESIAN_POINT('',(0.0211500000000099,-0.031,0.00160657243653548));
#31872=CARTESIAN_POINT('',(0.0211500000000044,-0.03075,0.00793218971944469));
#31873=CARTESIAN_POINT('',(0.0211500000000044,-0.024,0.00793218971944469));
#31874=CARTESIAN_POINT('',(0.0211500000000043,-0.03074999999999,0.00800000000001137));
#31875=CARTESIAN_POINT('',(0.0211500000000099,-0.03075,0.00160657243653548));
#31876=CARTESIAN_POINT('',(0.0211500000000043,-0.0275,0.008));
#31877=CARTESIAN_POINT('Origin',(0.02715,-0.024,-0.00793218971944484));
#31878=CARTESIAN_POINT('',(0.022500000000002,-0.03074999999999,-0.00793218971944484));
#31879=CARTESIAN_POINT('',(0.019075,-0.03075,-0.00793218971944484));
#31880=CARTESIAN_POINT('',(0.022500000000002,-0.031,-0.00793218971944484));
#31881=CARTESIAN_POINT('',(0.0225,-0.0275,-0.00793218971944484));
#31882=CARTESIAN_POINT('',(0.019075,-0.031,-0.00793218971944484));
#31883=CARTESIAN_POINT('Origin',(0.0211500000000044,-0.024,0.00793218971944473));
#31884=CARTESIAN_POINT('',(0.0225000000000178,-0.031,0.00793218971944473));
#31885=CARTESIAN_POINT('',(0.0160750000000022,-0.031,0.00793218971944473));
#31886=CARTESIAN_POINT('',(0.0225000000000178,-0.03074999999999,0.00793218971944473));
#31887=CARTESIAN_POINT('',(0.0225,-0.0275,0.00793218971944473));
#31888=CARTESIAN_POINT('',(0.0160750000000022,-0.03075,0.00793218971944473));
#31889=CARTESIAN_POINT('Origin',(0.0225,-0.031,-0.008));
#31890=CARTESIAN_POINT('',(0.0175,-0.031,-0.008));
#31891=CARTESIAN_POINT('',(0.0225000000000099,-0.031,-0.00800000000000999));
#31892=CARTESIAN_POINT('',(0.0175,-0.03075,-0.008));
#31893=CARTESIAN_POINT('',(0.01750000000001,-0.031,-0.00800000000000999));
#31894=CARTESIAN_POINT('',(0.0225000000000099,-0.03074999999999,-0.00800000000000999));
#31895=CARTESIAN_POINT('Origin',(0.011,-0.031,-0.00975));
#31896=CARTESIAN_POINT('',(0.0225000000000099,-0.031,-9.98512365149887E-15));
#31897=CARTESIAN_POINT('',(0.0175,-0.031,0.008));
#31898=CARTESIAN_POINT('',(0.0225000000000099,-0.031,0.00800000000001002));
#31899=CARTESIAN_POINT('',(0.0065,-0.031,0.0195));
#31900=CARTESIAN_POINT('',(0.01750000000001,-0.031,0.00800000000001001));
#31901=CARTESIAN_POINT('',(-0.000500000000000057,-0.031,0.0195));
#31902=CARTESIAN_POINT('',(0.00650000000000994,-0.031,0.01950000000001));
#31903=CARTESIAN_POINT('',(-0.000500000000000053,-0.031,0.0129903810567666));
#31904=CARTESIAN_POINT('',(-0.000500000000010059,-0.031,0.01950000000001));
#31905=CARTESIAN_POINT('',(-0.000500000000000034,-0.031,-0.0129903810567666));
#31906=CARTESIAN_POINT('Origin',(-4.35057343591877E-17,-0.031,8.02542624668979E-33));
#31907=CARTESIAN_POINT('',(-0.000500000000000036,-0.031,-0.0195));
#31908=CARTESIAN_POINT('',(-0.000500000000010036,-0.031,-0.01950000000001));
#31909=CARTESIAN_POINT('',(0.0065,-0.031,-0.0195));
#31910=CARTESIAN_POINT('',(0.00650000000000996,-0.031,-0.01950000000001));
#31911=CARTESIAN_POINT('',(0.01750000000001,-0.031,-0.00800000000000999));
#31912=CARTESIAN_POINT('Origin',(0.0225,-0.031,0.008));
#31913=CARTESIAN_POINT('',(0.0175,-0.03075,0.008));
#31914=CARTESIAN_POINT('',(0.0225000000000099,-0.03074999999999,0.00800000000001002));
#31915=CARTESIAN_POINT('',(0.01750000000001,-0.031,0.00800000000001001));
#31916=CARTESIAN_POINT('Origin',(-0.000500000000000057,-0.031,0.0195));
#31917=CARTESIAN_POINT('',(-0.000500000000000057,-0.03075,0.0195));
#31918=CARTESIAN_POINT('',(-0.000500000000010059,-0.031,0.01950000000001));
#31919=CARTESIAN_POINT('',(-0.000500000000000053,-0.03075,0.0129903810567666));
#31920=CARTESIAN_POINT('',(-0.000500000000010059,-0.03074999999999,0.01950000000001));
#31921=CARTESIAN_POINT('',(-0.000500000000010053,-0.031,0.0129903810567766));
#31922=CARTESIAN_POINT('Origin',(0.0065,-0.031,0.0195));
#31923=CARTESIAN_POINT('',(0.0065,-0.03075,0.0195));
#31924=CARTESIAN_POINT('',(0.00650000000000994,-0.031,0.01950000000001));
#31925=CARTESIAN_POINT('',(0.00650000000000994,-0.03074999999999,0.01950000000001));
#31926=CARTESIAN_POINT('Origin',(0.0175,-0.031,0.008));
#31927=CARTESIAN_POINT('',(0.01750000000001,-0.03074999999999,0.00800000000001001));
#31928=CARTESIAN_POINT('Origin',(0.0225,-0.031,1.48289771724852E-17));
#31929=CARTESIAN_POINT('',(0.0225000000000099,-0.03074999999999,-9.98512365149887E-15));
#31930=CARTESIAN_POINT('Origin',(-4.35057343591877E-17,-0.031,8.02542624668979E-33));
#31931=CARTESIAN_POINT('',(-0.000500000000000034,-0.03075,-0.0129903810567666));
#31932=CARTESIAN_POINT('Origin',(-4.35207874696186E-17,-0.03074999999999,
8.0332637042736E-33));
#31933=CARTESIAN_POINT('',(-0.000500000000010037,-0.031,-0.0129903810567766));
#31934=CARTESIAN_POINT('Origin',(-0.000500000000000036,-0.031,-0.0195));
#31935=CARTESIAN_POINT('',(-0.000500000000000037,-0.03075,-0.0195));
#31936=CARTESIAN_POINT('',(-0.000500000000010036,-0.03074999999999,-0.01950000000001));
#31937=CARTESIAN_POINT('',(-0.000500000000010036,-0.031,-0.01950000000001));
#31938=CARTESIAN_POINT('Origin',(0.0065,-0.031,-0.0195));
#31939=CARTESIAN_POINT('',(0.0065,-0.03075,-0.0195));
#31940=CARTESIAN_POINT('',(0.00650000000000996,-0.03074999999999,-0.01950000000001));
#31941=CARTESIAN_POINT('',(0.00650000000000996,-0.031,-0.01950000000001));
#31942=CARTESIAN_POINT('Origin',(0.0175,-0.031,-0.008));
#31943=CARTESIAN_POINT('',(0.01750000000001,-0.03074999999999,-0.00800000000000999));
#31944=CARTESIAN_POINT('Origin',(0.011,-0.03075,-0.00975));
#31945=CARTESIAN_POINT('',(0.,0.,0.));
#31946=CARTESIAN_POINT('Origin',(0.01765,-0.03005,-0.00731086937588517));
#31947=CARTESIAN_POINT('',(0.01765,-0.03005,-0.00806086937588517));
#31948=CARTESIAN_POINT('Origin',(0.01765000000001,-0.03005,-0.00731086937589517));
#31949=CARTESIAN_POINT('',(0.01765,-0.02924999999999,-0.00806086937588517));
#31950=CARTESIAN_POINT('',(0.01765,-0.03005,-0.00806086937588517));
#31951=CARTESIAN_POINT('Origin',(0.01765000000001,-0.02924999999999,-0.00731086937589517));
#31952=CARTESIAN_POINT('Origin',(0.01765,-0.03005,0.0073108693758851));
#31953=CARTESIAN_POINT('',(0.01765,-0.03005,0.0065608693758851));
#31954=CARTESIAN_POINT('Origin',(0.0176500000000099,-0.03005,0.0073108693758951));
#31955=CARTESIAN_POINT('',(0.01765,-0.02924999999999,0.0065608693758851));
#31956=CARTESIAN_POINT('',(0.01765,-0.03005,0.0065608693758851));
#31957=CARTESIAN_POINT('Origin',(0.0176500000000099,-0.02924999999999,0.0073108693758951));
#31958=CARTESIAN_POINT('Origin',(0.00731086937588504,-0.03005,-0.01765));
#31959=CARTESIAN_POINT('',(0.00731086937588504,-0.03005,-0.0184));
#31960=CARTESIAN_POINT('Origin',(0.00731086937589504,-0.03005,-0.0176500000000101));
#31961=CARTESIAN_POINT('',(0.00731086937588504,-0.02924999999999,-0.0184));
#31962=CARTESIAN_POINT('',(0.00731086937588504,-0.03005,-0.0184));
#31963=CARTESIAN_POINT('Origin',(0.00731086937589504,-0.02924999999999,
-0.0176500000000101));
#31964=CARTESIAN_POINT('Origin',(0.00731086937588512,-0.03005,0.01765));
#31965=CARTESIAN_POINT('',(0.00731086937588512,-0.03005,0.0169));
#31966=CARTESIAN_POINT('Origin',(0.00731086937589512,-0.03005,0.0176500000000099));
#31967=CARTESIAN_POINT('',(0.00731086937588512,-0.02924999999999,0.0169));
#31968=CARTESIAN_POINT('',(0.00731086937588512,-0.03005,0.0169));
#31969=CARTESIAN_POINT('Origin',(0.00731086937589512,-0.02924999999999,
0.0176500000000099));
#31970=CARTESIAN_POINT('Origin',(0.0209,-0.0744704599711237,0.005));
#31971=CARTESIAN_POINT('',(0.0209,-0.03005,0.0044));
#31972=CARTESIAN_POINT('Origin',(0.02090000000001,-0.03005,0.00500000000001));
#31973=CARTESIAN_POINT('',(0.0209,-0.02924999999999,0.0044));
#31974=CARTESIAN_POINT('',(0.0209,-0.0744704599711237,0.0044));
#31975=CARTESIAN_POINT('Origin',(0.02090000000001,-0.02924999999999,0.00500000000001));
#31976=CARTESIAN_POINT('Origin',(0.0209,-0.0744704599711237,0.003));
#31977=CARTESIAN_POINT('',(0.0209,-0.03005,0.0024));
#31978=CARTESIAN_POINT('Origin',(0.02090000000001,-0.03005,0.00300000000001001));
#31979=CARTESIAN_POINT('',(0.0209,-0.02924999999999,0.0024));
#31980=CARTESIAN_POINT('',(0.0209,-0.0744704599711237,0.0024));
#31981=CARTESIAN_POINT('Origin',(0.02090000000001,-0.02924999999999,0.00300000000001001));
#31982=CARTESIAN_POINT('Origin',(0.0209,-0.0744704599711237,0.001));
#31983=CARTESIAN_POINT('',(0.0209,-0.03005,0.000400000000000001));
#31984=CARTESIAN_POINT('Origin',(0.02090000000001,-0.03005,0.00100000000001));
#31985=CARTESIAN_POINT('',(0.0209,-0.02924999999999,0.000400000000000001));
#31986=CARTESIAN_POINT('',(0.0209,-0.0744704599711237,0.0004));
#31987=CARTESIAN_POINT('Origin',(0.02090000000001,-0.02924999999999,0.00100000000001));
#31988=CARTESIAN_POINT('Origin',(0.0209,-0.0744704599711237,-0.003));
#31989=CARTESIAN_POINT('',(0.0209,-0.03005,-0.0036));
#31990=CARTESIAN_POINT('Origin',(0.02090000000001,-0.03005,-0.00300000000001));
#31991=CARTESIAN_POINT('',(0.0209,-0.02924999999999,-0.0036));
#31992=CARTESIAN_POINT('',(0.0209,-0.0744704599711237,-0.0036));
#31993=CARTESIAN_POINT('Origin',(0.02090000000001,-0.02924999999999,-0.00300000000001));
#31994=CARTESIAN_POINT('Origin',(0.0209,-0.0744704599711237,-0.005));
#31995=CARTESIAN_POINT('',(0.0209,-0.03005,-0.0056));
#31996=CARTESIAN_POINT('Origin',(0.02090000000001,-0.03005,-0.00500000000001));
#31997=CARTESIAN_POINT('',(0.0209,-0.02924999999999,-0.0056));
#31998=CARTESIAN_POINT('',(0.0209,-0.0744704599711237,-0.0056));
#31999=CARTESIAN_POINT('Origin',(0.02090000000001,-0.02924999999999,-0.00500000000001));
#32000=CARTESIAN_POINT('Origin',(0.0209,-0.0744704599711237,-0.001));
#32001=CARTESIAN_POINT('',(0.0209,-0.03005,-0.0016));
#32002=CARTESIAN_POINT('Origin',(0.02090000000001,-0.03005,-0.00100000000001));
#32003=CARTESIAN_POINT('',(0.0209,-0.02924999999999,-0.0016));
#32004=CARTESIAN_POINT('',(0.0209,-0.0744704599711237,-0.0016));
#32005=CARTESIAN_POINT('Origin',(0.02090000000001,-0.02924999999999,-0.00100000000001));
#32006=CARTESIAN_POINT('Origin',(0.0199,-0.03005,0.0071));
#32007=CARTESIAN_POINT('',(0.0199,-0.03005,0.0071));
#32008=CARTESIAN_POINT('',(0.0079000000000001,-0.03005,0.019));
#32009=CARTESIAN_POINT('',(0.0199000000000101,-0.03005,0.00710000000001001));
#32010=CARTESIAN_POINT('',(0.0199,-0.02925,0.0071));
#32011=CARTESIAN_POINT('',(0.0199000000000101,-0.03005,0.00710000000001001));
#32012=CARTESIAN_POINT('',(0.0079000000000001,-0.02925,0.019));
#32013=CARTESIAN_POINT('',(0.0199000000000101,-0.02924999999999,0.00710000000001001));
#32014=CARTESIAN_POINT('',(0.00790000000001011,-0.03005,0.0190000000000101));
#32015=CARTESIAN_POINT('Origin',(0.0264,-0.03005,0.0071));
#32016=CARTESIAN_POINT('',(0.0264,-0.03005,0.0071));
#32017=CARTESIAN_POINT('',(0.0264000000000101,-0.03005,0.00710000000000998));
#32018=CARTESIAN_POINT('',(0.0264,-0.02925,0.0071));
#32019=CARTESIAN_POINT('',(0.0264000000000101,-0.03005,0.00710000000000998));
#32020=CARTESIAN_POINT('',(0.0264000000000101,-0.02924999999999,0.00710000000000998));
#32021=CARTESIAN_POINT('Origin',(0.0019000000000001,-0.03005,0.019));
#32022=CARTESIAN_POINT('',(0.0019000000000001,-0.03005,0.019));
#32023=CARTESIAN_POINT('',(0.00190000000000008,-0.03005,0.0136930639376293));
#32024=CARTESIAN_POINT('',(0.00190000000001011,-0.03005,0.0190000000000101));
#32025=CARTESIAN_POINT('',(0.0019000000000001,-0.02925,0.019));
#32026=CARTESIAN_POINT('',(0.00190000000001011,-0.03005,0.0190000000000101));
#32027=CARTESIAN_POINT('',(0.00190000000000008,-0.02925,0.0136930639376293));
#32028=CARTESIAN_POINT('',(0.00190000000001011,-0.02924999999999,0.0190000000000101));
#32029=CARTESIAN_POINT('',(0.00190000000001009,-0.03005,0.0136930639376393));
#32030=CARTESIAN_POINT('Origin',(0.0079000000000001,-0.03005,0.019));
#32031=CARTESIAN_POINT('',(0.00790000000001011,-0.03005,0.0190000000000101));
#32032=CARTESIAN_POINT('',(0.00790000000001011,-0.02924999999999,0.0190000000000101));
#32033=CARTESIAN_POINT('Origin',(0.0199,-0.03005,-0.0071));
#32034=CARTESIAN_POINT('',(0.0199,-0.03005,-0.0071));
#32035=CARTESIAN_POINT('',(0.0079,-0.03005,-0.019));
#32036=CARTESIAN_POINT('',(0.01990000000001,-0.03005,-0.00710000000000999));
#32037=CARTESIAN_POINT('',(0.0079,-0.02925,-0.019));
#32038=CARTESIAN_POINT('',(0.00790000000000993,-0.03005,-0.0190000000000099));
#32039=CARTESIAN_POINT('',(0.0199,-0.02925,-0.0071));
#32040=CARTESIAN_POINT('',(0.01990000000001,-0.02924999999999,-0.00710000000000999));
#32041=CARTESIAN_POINT('',(0.01990000000001,-0.03005,-0.00710000000000999));
#32042=CARTESIAN_POINT('Origin',(0.0264,-0.03005,-0.0071));
#32043=CARTESIAN_POINT('',(0.0264,-0.03005,-0.0071));
#32044=CARTESIAN_POINT('',(0.02640000000001,-0.03005,-0.00710000000001002));
#32045=CARTESIAN_POINT('',(0.0264,-0.02925,-0.0071));
#32046=CARTESIAN_POINT('',(0.02640000000001,-0.02924999999999,-0.00710000000001002));
#32047=CARTESIAN_POINT('',(0.02640000000001,-0.03005,-0.00710000000001002));
#32048=CARTESIAN_POINT('Origin',(0.0264,-0.03005,-2.31739922485765E-17));
#32049=CARTESIAN_POINT('',(0.02640000000001,-0.03005,-1.00231739922486E-14));
#32050=CARTESIAN_POINT('',(0.02640000000001,-0.02924999999999,-1.00231669383767E-14));
#32051=CARTESIAN_POINT('Origin',(0.000650000000000017,-0.03005,9.37463700322586E-17));
#32052=CARTESIAN_POINT('',(0.00189999999999995,-0.03005,-0.0136930639376291));
#32053=CARTESIAN_POINT('Origin',(0.000650000000000017,-0.03005,9.37463700322586E-17));
#32054=CARTESIAN_POINT('',(0.00189999999999995,-0.02925,-0.0136930639376291));
#32055=CARTESIAN_POINT('Origin',(0.000650000000000017,-0.02924999999999,
9.37534239041485E-17));
#32056=CARTESIAN_POINT('',(0.00190000000000995,-0.03005,-0.0136930639376391));
#32057=CARTESIAN_POINT('Origin',(0.00189999999999993,-0.03005,-0.019));
#32058=CARTESIAN_POINT('',(0.00189999999999993,-0.03005,-0.019));
#32059=CARTESIAN_POINT('',(0.00190000000000993,-0.03005,-0.0190000000000099));
#32060=CARTESIAN_POINT('',(0.00189999999999993,-0.02925,-0.019));
#32061=CARTESIAN_POINT('',(0.00190000000000993,-0.02924999999999,-0.0190000000000099));
#32062=CARTESIAN_POINT('',(0.00190000000000993,-0.03005,-0.0190000000000099));
#32063=CARTESIAN_POINT('Origin',(0.0079,-0.03005,-0.019));
#32064=CARTESIAN_POINT('',(0.00790000000000993,-0.03005,-0.0190000000000099));
#32065=CARTESIAN_POINT('',(0.00790000000000993,-0.02924999999999,-0.0190000000000099));
#32066=CARTESIAN_POINT('Origin',(0.01415,-0.02925,-0.0095));
#32067=CARTESIAN_POINT('Origin',(0.01415,-0.03005,-0.0095));
#32068=CARTESIAN_POINT('',(0.,0.,0.));
#32069=CARTESIAN_POINT('Origin',(0.02115,-0.0223,-0.01175));
#32070=CARTESIAN_POINT('',(0.02115,-0.02545,-0.00325000000000007));
#32071=CARTESIAN_POINT('',(0.02115,-0.02545,-0.00275000000000007));
#32072=CARTESIAN_POINT('',(0.0211500000000101,-0.02545000000001,-0.00749999999999003));
#32073=CARTESIAN_POINT('',(0.02115,-0.0317,-0.00275000000000007));
#32074=CARTESIAN_POINT('',(0.0211500000000101,-0.02545000000001,-0.00274999999999008));
#32075=CARTESIAN_POINT('',(0.02115,-0.0317,-0.00325000000000007));
#32076=CARTESIAN_POINT('',(0.0211500000000101,-0.0317000000000099,-0.00549999999999003));
#32077=CARTESIAN_POINT('',(0.02115000000001,-0.02545000000001,-0.00324999999999007));
#32078=CARTESIAN_POINT('Origin',(0.02115,-0.0317,0.000749999999999928));
#32079=CARTESIAN_POINT('',(0.02065,-0.0317,-0.00275000000000007));
#32080=CARTESIAN_POINT('',(0.0206500000000101,-0.03170000000001,-0.00274999999999007));
#32081=CARTESIAN_POINT('',(0.02065,-0.0317,-0.00325000000000006));
#32082=CARTESIAN_POINT('',(0.0206500000000101,-0.03170000000001,-0.00274999999999007));
#32083=CARTESIAN_POINT('',(0.0206500000000101,-0.03170000000001,-0.00324999999999008));
#32084=CARTESIAN_POINT('Origin',(0.02115,-0.02545,-0.00300000000000007));
#32085=CARTESIAN_POINT('',(0.02115,-0.02495,-0.00325000000000007));
#32086=CARTESIAN_POINT('',(0.02115,-0.02495,-0.00275000000000007));
#32087=CARTESIAN_POINT('',(0.0211500000000101,-0.02495000000001,-0.00274999999999008));
#32088=CARTESIAN_POINT('',(0.02065,-0.02545,-0.00325000000000006));
#32089=CARTESIAN_POINT('Origin',(0.02115000000001,-0.02545000000001,-0.00324999999999007));
#32090=CARTESIAN_POINT('',(0.02065,-0.02545,-0.00275000000000007));
#32091=CARTESIAN_POINT('',(0.0206500000000101,-0.02545000000001,-0.00274999999999008));
#32092=CARTESIAN_POINT('Origin',(0.0211500000000101,-0.02545000000001,-0.00274999999999008));
#32093=CARTESIAN_POINT('Origin',(0.02065,-0.02545,-0.00275000000000007));
#32094=CARTESIAN_POINT('',(0.0206500000000101,-0.02545000000001,-0.00324999999999008));
#32095=CARTESIAN_POINT('',(0.0206500000000101,-0.02545000000001,-0.00274999999999008));
#32096=CARTESIAN_POINT('Origin',(0.0229,-0.02495,-0.00325000000000009));
#32097=CARTESIAN_POINT('',(0.0262,-0.02495,-0.00275000000000013));
#32098=CARTESIAN_POINT('',(0.0229000000000101,-0.02495000000001,-0.00274999999999008));
#32099=CARTESIAN_POINT('',(0.0262,-0.02495,-0.00325000000000012));
#32100=CARTESIAN_POINT('',(0.0262000000000101,-0.02495000000001,-0.00274999999999007));
#32101=CARTESIAN_POINT('',(0.0229000000000101,-0.02495000000001,-0.00324999999999007));
#32102=CARTESIAN_POINT('Origin',(0.0229,-0.02545,-0.00325000000000009));
#32103=CARTESIAN_POINT('',(0.0262,-0.02545,-0.00325000000000012));
#32104=CARTESIAN_POINT('',(0.0262000000000101,-0.02495000000001,-0.00324999999999008));
#32105=CARTESIAN_POINT('',(0.0229000000000101,-0.02545000000001,-0.00324999999999007));
#32106=CARTESIAN_POINT('Origin',(0.0229,-0.02545,-0.00275000000000009));
#32107=CARTESIAN_POINT('',(0.0262,-0.02545,-0.00275000000000013));
#32108=CARTESIAN_POINT('',(0.0262000000000101,-0.02545000000001,-0.00324999999999008));
#32109=CARTESIAN_POINT('',(0.0229000000000101,-0.02545000000001,-0.00274999999999008));
#32110=CARTESIAN_POINT('Origin',(0.0229,-0.02495,-0.00275000000000009));
#32111=CARTESIAN_POINT('',(0.0262000000000101,-0.02545000000001,-0.00274999999999008));
#32112=CARTESIAN_POINT('Origin',(0.0262,-0.0252,-0.00300000000000012));
#32113=CARTESIAN_POINT('',(0.,0.,0.));
#32114=CARTESIAN_POINT('Origin',(-0.00643329000430782,-0.008,-0.0115261780187742));
#32115=CARTESIAN_POINT('',(-0.00621272270841107,-0.008,-0.011643864330556));
#32116=CARTESIAN_POINT('',(-0.00655513261802576,-0.008,-0.0117444768448874));
#32117=CARTESIAN_POINT('Origin',(-0.00643329000431782,-0.00799999999999,
-0.0115261780187842));
#32118=CARTESIAN_POINT('',(-0.00655513261802576,-0.024,-0.0117444768448874));
#32119=CARTESIAN_POINT('',(-0.00655513261803576,-0.00799999999999,-0.0117444768448974));
#32120=CARTESIAN_POINT('',(-0.00621272270841107,-0.024,-0.011643864330556));
#32121=CARTESIAN_POINT('Origin',(-0.00643329000431782,-0.02400000000001,
-0.0115261780187842));
#32122=CARTESIAN_POINT('',(-0.00621272270842108,-0.00799999999999,-0.011643864330566));
#32123=CARTESIAN_POINT('Origin',(-4.44089209850063E-17,-0.008,6.72997231505748E-33));
#32124=CARTESIAN_POINT('',(-0.00689344899281775,-0.008,-0.0115491497948299));
#32125=CARTESIAN_POINT('Origin',(-4.44089209850063E-17,-0.00799999999999,
6.72997231505748E-33));
#32126=CARTESIAN_POINT('',(-0.00689344899281775,-0.024,-0.0115491497948299));
#32127=CARTESIAN_POINT('',(-0.00689344899282776,-0.00799999999999,-0.0115491497948399));
#32128=CARTESIAN_POINT('Origin',(-4.44089209850063E-17,-0.02400000000001,
6.72997231505748E-33));
#32129=CARTESIAN_POINT('Origin',(-0.00676531797064642,-0.008,-0.0113344815830301));
#32130=CARTESIAN_POINT('',(-0.0069775209542755,-0.008,-0.0112023078574304));
#32131=CARTESIAN_POINT('Origin',(-0.00676531797065643,-0.00799999999999,
-0.0113344815830401));
#32132=CARTESIAN_POINT('',(-0.0069775209542755,-0.024,-0.0112023078574304));
#32133=CARTESIAN_POINT('',(-0.0069775209542855,-0.00799999999999,-0.0112023078574404));
#32134=CARTESIAN_POINT('Origin',(-0.00676531797065643,-0.02400000000001,
-0.0113344815830401));
#32135=CARTESIAN_POINT('Origin',(-0.00687303373118612,-0.008,-0.0110345551487125));
#32136=CARTESIAN_POINT('',(-0.00687303373118612,-0.008,-0.0110345551487125));
#32137=CARTESIAN_POINT('',(-0.00673974017575294,-0.00799999999999,-0.0108205542946554));
#32138=CARTESIAN_POINT('',(-0.00687303373118612,-0.024,-0.0110345551487125));
#32139=CARTESIAN_POINT('',(-0.00687303373119612,-0.016,-0.0110345551487225));
#32140=CARTESIAN_POINT('',(-0.00673974017575294,-0.02400000000001,-0.0108205542946554));
#32141=CARTESIAN_POINT('Origin',(-0.00788272044413954,-0.008,-0.0105878571202838));
#32142=CARTESIAN_POINT('',(-0.00767940127818889,-0.008,-0.0107333264186156));
#32143=CARTESIAN_POINT('',(-0.00803201439194522,-0.008,-0.0107883847172589));
#32144=CARTESIAN_POINT('Origin',(-0.00788272044414955,-0.00799999999999,
-0.0105878571202938));
#32145=CARTESIAN_POINT('',(-0.00803201439194522,-0.024,-0.0107883847172589));
#32146=CARTESIAN_POINT('',(-0.00803201439195522,-0.00799999999999,-0.0107883847172689));
#32147=CARTESIAN_POINT('',(-0.00767940127818889,-0.024,-0.0107333264186156));
#32148=CARTESIAN_POINT('Origin',(-0.00788272044414955,-0.02400000000001,
-0.0105878571202938));
#32149=CARTESIAN_POINT('',(-0.00767940127819889,-0.00799999999999,-0.0107333264186256));
#32150=CARTESIAN_POINT('Origin',(-4.44089209850063E-17,-0.008,6.72997231505748E-33));
#32151=CARTESIAN_POINT('',(-0.00834194112716978,-0.008,-0.0105505695690249));
#32152=CARTESIAN_POINT('Origin',(-4.44089209850063E-17,-0.00799999999999,
6.72997231505748E-33));
#32153=CARTESIAN_POINT('',(-0.00834194112716978,-0.024,-0.0105505695690249));
#32154=CARTESIAN_POINT('',(-0.00834194112717978,-0.00799999999999,-0.0105505695690349));
#32155=CARTESIAN_POINT('Origin',(-4.44089209850063E-17,-0.02400000000001,
6.72997231505748E-33));
#32156=CARTESIAN_POINT('Origin',(-0.00818688645937852,-0.008,-0.010354462327965));
#32157=CARTESIAN_POINT('',(-0.00838002188395169,-0.008,-0.0101957213194796));
#32158=CARTESIAN_POINT('Origin',(-0.00818688645938851,-0.00799999999999,
-0.010354462327975));
#32159=CARTESIAN_POINT('',(-0.00838002188395169,-0.024,-0.0101957213194796));
#32160=CARTESIAN_POINT('',(-0.0083800218839617,-0.00799999999999,-0.0101957213194896));
#32161=CARTESIAN_POINT('Origin',(-0.00818688645938851,-0.02400000000001,
-0.010354462327975));
#32162=CARTESIAN_POINT('Origin',(-0.00825453244123697,-0.008,-0.0100430420778053));
#32163=CARTESIAN_POINT('',(-0.00825453244123697,-0.008,-0.0100430420778053));
#32164=CARTESIAN_POINT('',(-0.00818084247458025,-0.00799999999999,-0.0099533857052449));
#32165=CARTESIAN_POINT('',(-0.00825453244123697,-0.024,-0.0100430420778053));
#32166=CARTESIAN_POINT('',(-0.00825453244124697,-0.016,-0.0100430420778153));
#32167=CARTESIAN_POINT('',(-0.00818084247458025,-0.02400000000001,-0.0099533857052449));
#32168=CARTESIAN_POINT('Origin',(-0.00919727535166904,-0.008,-0.00946837505095685));
#32169=CARTESIAN_POINT('',(-0.00901468316296463,-0.008,-0.00963913831581242));
#32170=CARTESIAN_POINT('',(-0.00937146617272338,-0.008,-0.00964770033601285));
#32171=CARTESIAN_POINT('Origin',(-0.00919727535167904,-0.00799999999999,
-0.00946837505096685));
#32172=CARTESIAN_POINT('',(-0.00937146617272338,-0.024,-0.00964770033601285));
#32173=CARTESIAN_POINT('',(-0.00937146617273337,-0.00799999999999,-0.00964770033602285));
#32174=CARTESIAN_POINT('',(-0.00901468316296463,-0.024,-0.00963913831581242));
#32175=CARTESIAN_POINT('Origin',(-0.00919727535167904,-0.02400000000001,
-0.00946837505096685));
#32176=CARTESIAN_POINT('',(-0.00901468316297463,-0.00799999999999,-0.00963913831582242));
#32177=CARTESIAN_POINT('Origin',(-4.44089209850063E-17,-0.008,6.72997231505748E-33));
#32178=CARTESIAN_POINT('',(-0.00964770033601289,-0.008,-0.00937146617272333));
#32179=CARTESIAN_POINT('Origin',(-4.44089209850063E-17,-0.00799999999999,
6.72997231505748E-33));
#32180=CARTESIAN_POINT('',(-0.00964770033601289,-0.024,-0.00937146617272333));
#32181=CARTESIAN_POINT('',(-0.0096477003360229,-0.00799999999999,-0.00937146617273333));
#32182=CARTESIAN_POINT('Origin',(-4.44089209850063E-17,-0.02400000000001,
6.72997231505748E-33));
#32183=CARTESIAN_POINT('Origin',(-0.00946837505095689,-0.008,-0.00919727535166899));
#32184=CARTESIAN_POINT('',(-0.00963913831581246,-0.008,-0.00901468316296458));
#32185=CARTESIAN_POINT('Origin',(-0.00946837505096689,-0.00799999999999,
-0.00919727535167899));
#32186=CARTESIAN_POINT('',(-0.00963913831581246,-0.024,-0.00901468316296458));
#32187=CARTESIAN_POINT('',(-0.00963913831582247,-0.00799999999999,-0.00901468316297458));
#32188=CARTESIAN_POINT('Origin',(-0.00946837505096689,-0.02400000000001,
-0.00919727535167899));
#32189=CARTESIAN_POINT('Origin',(-0.00949479381262948,-0.008,-0.00887968977248946));
#32190=CARTESIAN_POINT('',(-0.00949479381262948,-0.008,-0.00887968977248946));
#32191=CARTESIAN_POINT('',(-0.00942962993438211,-0.00799999999999,-0.00881874742507027));
#32192=CARTESIAN_POINT('',(-0.00949479381262948,-0.024,-0.00887968977248946));
#32193=CARTESIAN_POINT('',(-0.00949479381263948,-0.016,-0.00887968977249946));
#32194=CARTESIAN_POINT('',(-0.00942962993438211,-0.02400000000001,-0.00881874742507027));
#32195=CARTESIAN_POINT('Origin',(-0.010354462327965,-0.008,-0.00818688645937847));
#32196=CARTESIAN_POINT('',(-0.0101957213194796,-0.008,-0.00838002188395165));
#32197=CARTESIAN_POINT('',(-0.0105505695690249,-0.008,-0.00834194112716973));
#32198=CARTESIAN_POINT('Origin',(-0.010354462327975,-0.00799999999999,-0.00818688645938847));
#32199=CARTESIAN_POINT('',(-0.0105505695690249,-0.024,-0.00834194112716973));
#32200=CARTESIAN_POINT('',(-0.0105505695690349,-0.00799999999999,-0.00834194112717973));
#32201=CARTESIAN_POINT('',(-0.0101957213194796,-0.024,-0.00838002188395165));
#32202=CARTESIAN_POINT('Origin',(-0.010354462327975,-0.02400000000001,-0.00818688645938847));
#32203=CARTESIAN_POINT('',(-0.0101957213194896,-0.00799999999999,-0.00838002188396165));
#32204=CARTESIAN_POINT('Origin',(-4.44089209850063E-17,-0.008,6.72997231505748E-33));
#32205=CARTESIAN_POINT('',(-0.0107883847172589,-0.008,-0.00803201439194517));
#32206=CARTESIAN_POINT('Origin',(-4.44089209850063E-17,-0.00799999999999,
6.72997231505748E-33));
#32207=CARTESIAN_POINT('',(-0.0107883847172589,-0.024,-0.00803201439194517));
#32208=CARTESIAN_POINT('',(-0.0107883847172689,-0.00799999999999,-0.00803201439195516));
#32209=CARTESIAN_POINT('Origin',(-4.44089209850063E-17,-0.02400000000001,
6.72997231505748E-33));
#32210=CARTESIAN_POINT('Origin',(-0.0105878571202839,-0.008,-0.00788272044413949));
#32211=CARTESIAN_POINT('',(-0.0107333264186156,-0.008,-0.00767940127818885));
#32212=CARTESIAN_POINT('Origin',(-0.0105878571202939,-0.00799999999999,
-0.00788272044414949));
#32213=CARTESIAN_POINT('',(-0.0107333264186156,-0.024,-0.00767940127818885));
#32214=CARTESIAN_POINT('',(-0.0107333264186256,-0.00799999999999,-0.00767940127819885));
#32215=CARTESIAN_POINT('Origin',(-0.0105878571202939,-0.02400000000001,
-0.00788272044414949));
#32216=CARTESIAN_POINT('Origin',(-0.0105725966294337,-0.008,-0.00756440351325123));
#32217=CARTESIAN_POINT('',(-0.0105725966294337,-0.008,-0.00756440351325123));
#32218=CARTESIAN_POINT('',(-0.0104326500269426,-0.00799999999999,-0.00746427554955177));
#32219=CARTESIAN_POINT('',(-0.0105725966294337,-0.024,-0.00756440351325123));
#32220=CARTESIAN_POINT('',(-0.0105725966294437,-0.016,-0.00756440351326123));
#32221=CARTESIAN_POINT('',(-0.0104326500269426,-0.02400000000001,-0.00746427554955177));
#32222=CARTESIAN_POINT('Origin',(-0.0113344815830301,-0.008,-0.00676531797064638));
#32223=CARTESIAN_POINT('',(-0.0112023078574304,-0.008,-0.00697752095427546));
#32224=CARTESIAN_POINT('',(-0.0115491497948299,-0.008,-0.00689344899281771));
#32225=CARTESIAN_POINT('Origin',(-0.0113344815830401,-0.00799999999999,
-0.00676531797065638));
#32226=CARTESIAN_POINT('',(-0.0115491497948299,-0.024,-0.00689344899281771));
#32227=CARTESIAN_POINT('',(-0.0115491497948399,-0.00799999999999,-0.00689344899282771));
#32228=CARTESIAN_POINT('',(-0.0112023078574304,-0.024,-0.00697752095427546));
#32229=CARTESIAN_POINT('Origin',(-0.0113344815830401,-0.02400000000001,
-0.00676531797065638));
#32230=CARTESIAN_POINT('',(-0.0112023078574404,-0.00799999999999,-0.00697752095428546));
#32231=CARTESIAN_POINT('Origin',(-4.44089209850063E-17,-0.008,6.72997231505748E-33));
#32232=CARTESIAN_POINT('',(-0.0117444768448874,-0.008,-0.00655513261802572));
#32233=CARTESIAN_POINT('Origin',(-4.44089209850063E-17,-0.00799999999999,
6.72997231505748E-33));
#32234=CARTESIAN_POINT('',(-0.0117444768448874,-0.024,-0.00655513261802572));
#32235=CARTESIAN_POINT('',(-0.0117444768448974,-0.00799999999999,-0.00655513261803572));
#32236=CARTESIAN_POINT('Origin',(-4.44089209850063E-17,-0.02400000000001,
6.72997231505748E-33));
#32237=CARTESIAN_POINT('Origin',(-0.0115261780187742,-0.008,-0.00643329000430777));
#32238=CARTESIAN_POINT('',(-0.011643864330556,-0.008,-0.00621272270841103));
#32239=CARTESIAN_POINT('Origin',(-0.0115261780187842,-0.00799999999999,
-0.00643329000431777));
#32240=CARTESIAN_POINT('',(-0.011643864330556,-0.024,-0.00621272270841103));
#32241=CARTESIAN_POINT('',(-0.011643864330566,-0.00799999999999,-0.00621272270842103));
#32242=CARTESIAN_POINT('Origin',(-0.0115261780187842,-0.02400000000001,
-0.00643329000431777));
#32243=CARTESIAN_POINT('Origin',(-0.0114694993866308,-0.008,-0.0061196882126524));
#32244=CARTESIAN_POINT('',(-0.0114694993866308,-0.008,-0.0061196882126524));
#32245=CARTESIAN_POINT('',(-0.0111490530784194,-0.00799999999999,-0.00594871026243939));
#32246=CARTESIAN_POINT('',(-0.0114694993866308,-0.024,-0.0061196882126524));
#32247=CARTESIAN_POINT('',(-0.0114694993866408,-0.016,-0.0061196882126624));
#32248=CARTESIAN_POINT('',(-0.0111490530784194,-0.02400000000001,-0.00594871026243939));
#32249=CARTESIAN_POINT('Origin',(-0.0114165205192449,-0.008,-0.00711094643726559));
#32250=CARTESIAN_POINT('',(-0.0110345551487125,-0.024,-0.00687303373118608));
#32251=CARTESIAN_POINT('',(-0.0110115369799216,-0.02400000000001,-0.00685869652879265));
#32252=CARTESIAN_POINT('',(-0.0110345551487125,-0.008,-0.00687303373118608));
#32253=CARTESIAN_POINT('',(-0.0110345551487225,-0.016,-0.00687303373119608));
#32254=CARTESIAN_POINT('',(-0.0110115369799216,-0.00799999999999,-0.00685869652879265));
#32255=CARTESIAN_POINT('Origin',(-0.010390685842037,-0.008,-0.0085402662565105));
#32256=CARTESIAN_POINT('',(-0.0100430420778053,-0.024,-0.00825453244123691));
#32257=CARTESIAN_POINT('',(-0.0101272075873608,-0.02400000000001,-0.008323709382217));
#32258=CARTESIAN_POINT('',(-0.0100430420778053,-0.008,-0.00825453244123691));
#32259=CARTESIAN_POINT('',(-0.0100430420778153,-0.016,-0.00825453244124691));
#32260=CARTESIAN_POINT('',(-0.0101272075873608,-0.00799999999999,-0.008323709382217));
#32261=CARTESIAN_POINT('Origin',(-0.00782624825024844,-0.008,-0.0109385711281449));
#32262=CARTESIAN_POINT('',(-0.00756440351325127,-0.024,-0.0105725966294337));
#32263=CARTESIAN_POINT('',(-0.0075951979180504,-0.02400000000001,-0.0106156372762982));
#32264=CARTESIAN_POINT('',(-0.00756440351325127,-0.008,-0.0105725966294337));
#32265=CARTESIAN_POINT('',(-0.00756440351326127,-0.016,-0.0105725966294437));
#32266=CARTESIAN_POINT('',(-0.0075951979180504,-0.00799999999999,-0.0106156372762982));
#32267=CARTESIAN_POINT('Origin',(-0.00633152357385964,-0.008,-0.0118665205192449));
#32268=CARTESIAN_POINT('',(-0.00611968821265244,-0.024,-0.0114694993866308));
#32269=CARTESIAN_POINT('',(-0.00605462794304303,-0.02400000000001,-0.0113475636447265));
#32270=CARTESIAN_POINT('',(-0.00611968821265244,-0.008,-0.0114694993866308));
#32271=CARTESIAN_POINT('',(-0.00611968821266244,-0.016,-0.0114694993866408));
#32272=CARTESIAN_POINT('',(-0.00605462794304303,-0.00799999999999,-0.0113475636447265));
#32273=CARTESIAN_POINT('Origin',(-4.44089209850063E-17,-0.016,6.72997231505748E-33));
#32274=CARTESIAN_POINT('',(-0.0117336086965482,-0.008,-0.00559664425850784));
#32275=CARTESIAN_POINT('Origin',(-4.44089209850063E-17,-0.00799999999999,
6.72997231505748E-33));
#32276=CARTESIAN_POINT('',(-0.0117336086965482,-0.024,-0.00559664425850784));
#32277=CARTESIAN_POINT('',(-0.0117336086965582,-0.016,-0.00559664425851784));
#32278=CARTESIAN_POINT('Origin',(-4.44089209850063E-17,-0.02400000000001,
6.72997231505748E-33));
#32279=CARTESIAN_POINT('Origin',(-4.44089209850063E-17,-0.016,6.72997231505748E-33));
#32280=CARTESIAN_POINT('Origin',(-4.44089209850063E-17,-0.02400000000001,
6.72997231505748E-33));
#32281=CARTESIAN_POINT('Origin',(-4.44089209850063E-17,-0.00799999999999,
6.72997231505748E-33));
#32282=CARTESIAN_POINT('Origin',(-0.0090712898554855,-0.024,-0.00907128985548545));
#32283=CARTESIAN_POINT('',(-0.0125459354524631,-0.024,-0.00598410424563531));
#32284=CARTESIAN_POINT('',(-0.0125459354524731,-0.02400000000001,-0.00598410424564531));
#32285=CARTESIAN_POINT('',(-0.00598410424563535,-0.024,-0.0125459354524631));
#32286=CARTESIAN_POINT('Origin',(-4.44089209850063E-17,-0.02400000000001,
6.72997231505748E-33));
#32287=CARTESIAN_POINT('',(-0.00559664425850789,-0.024,-0.0117336086965482));
#32288=CARTESIAN_POINT('',(-0.00559664425851789,-0.02400000000001,-0.0117336086965582));
#32289=CARTESIAN_POINT('Origin',(-4.44089209850063E-17,-0.02400000000001,
6.72997231505748E-33));
#32290=CARTESIAN_POINT('Origin',(-4.44089209850063E-17,-0.02400000000001,
6.72997231505748E-33));
#32291=CARTESIAN_POINT('',(-0.0088796897724895,-0.024,-0.00949479381262943));
#32292=CARTESIAN_POINT('Origin',(-4.44089209850063E-17,-0.02400000000001,
6.72997231505748E-33));
#32293=CARTESIAN_POINT('',(-0.00897243436344032,-0.02400000000001,-0.00959396290421603));
#32294=CARTESIAN_POINT('Origin',(-4.44089209850063E-17,-0.02400000000001,
6.72997231505748E-33));
#32295=CARTESIAN_POINT('Origin',(-4.44089209850063E-17,-0.016,6.72997231505748E-33));
#32296=CARTESIAN_POINT('',(-0.0088796897724895,-0.008,-0.00949479381262943));
#32297=CARTESIAN_POINT('Origin',(-4.44089209850063E-17,-0.00799999999999,
6.72997231505748E-33));
#32298=CARTESIAN_POINT('',(-0.00887968977249951,-0.016,-0.00949479381263943));
#32299=CARTESIAN_POINT('Origin',(-4.44089209850063E-17,-0.016,6.72997231505748E-33));
#32300=CARTESIAN_POINT('',(-0.00559664425850789,-0.008,-0.0117336086965482));
#32301=CARTESIAN_POINT('',(-0.00559664425851789,-0.016,-0.0117336086965582));
#32302=CARTESIAN_POINT('Origin',(-4.44089209850063E-17,-0.00799999999999,
6.72997231505748E-33));
#32303=CARTESIAN_POINT('Origin',(-0.00918706364922952,-0.008,-0.00982345975229737));
#32304=CARTESIAN_POINT('',(-0.00897243436344032,-0.00799999999999,-0.00959396290421603));
#32305=CARTESIAN_POINT('Origin',(-4.44089209850063E-17,-0.016,6.72997231505748E-33));
#32306=CARTESIAN_POINT('Origin',(-4.44089209850063E-17,-0.00799999999999,
6.72997231505748E-33));
#32307=CARTESIAN_POINT('Origin',(-4.44089209850063E-17,-0.016,6.72997231505748E-33));
#32308=CARTESIAN_POINT('',(-0.0125459354524631,-0.008,-0.00598410424563531));
#32309=CARTESIAN_POINT('',(-0.0125459354524731,-0.016,-0.00598410424564531));
#32310=CARTESIAN_POINT('',(-0.00598410424563535,-0.008,-0.0125459354524631));
#32311=CARTESIAN_POINT('Origin',(-4.44089209850063E-17,-0.00799999999999,
6.72997231505748E-33));
#32312=CARTESIAN_POINT('',(-0.00598410424564535,-0.016,-0.0125459354524731));
#32313=CARTESIAN_POINT('Origin',(-0.00559664425850789,-0.016,-0.0117336086965482));
#32314=CARTESIAN_POINT('',(-0.00559664425851789,-0.00799999999999,-0.0117336086965582));
#32315=CARTESIAN_POINT('Origin',(-4.44089209850063E-17,-0.016,6.72997231505748E-33));
#32316=CARTESIAN_POINT('Origin',(-4.44089209850063E-17,-0.00799999999999,
6.72997231505748E-33));
#32317=CARTESIAN_POINT('Origin',(-0.0125459354524631,-0.016,-0.00598410424563531));
#32318=CARTESIAN_POINT('',(-0.0125459354524731,-0.00799999999999,-0.00598410424564531));
#32319=CARTESIAN_POINT('Origin',(-0.0090712898554855,-0.008,-0.00907128985548545));
#32320=CARTESIAN_POINT('',(0.,0.,0.));
#32321=CARTESIAN_POINT('Origin',(-4.59950432489715E-17,-0.01,1.1450674770076E-32));
#32322=CARTESIAN_POINT('',(0.00387499999999995,-0.01000000000001,-4.74550634669588E-19));
#32323=CARTESIAN_POINT('Origin',(-4.59950432489715E-17,-0.01000000000001,
1.1450674770076E-32));
#32324=CARTESIAN_POINT('',(-0.00250000000000005,-0.01000000000001,3.0616169978685E-19));
#32325=CARTESIAN_POINT('Origin',(-4.59950432489715E-17,-0.01000000000001,
1.1450674770076E-32));
#32326=CARTESIAN_POINT('Origin',(-4.59950432489715E-17,-0.0085,1.1450674770076E-32));
#32327=CARTESIAN_POINT('',(-0.00250000000000005,-0.00699999999999,3.0616169978685E-19));
#32328=CARTESIAN_POINT('',(-0.00250000000000005,-0.0085,3.0616169978685E-19));
#32329=CARTESIAN_POINT('Origin',(-4.59950432489715E-17,-0.00699999999999,
1.1450674770076E-32));
#32330=CARTESIAN_POINT('Origin',(-4.59950432489715E-17,-0.0085,1.1450674770076E-32));
#32331=CARTESIAN_POINT('',(0.00387499999999995,-0.00699999999999,-4.74550634669588E-19));
#32332=CARTESIAN_POINT('Origin',(-4.59950432489715E-17,-0.00699999999999,
1.1450674770076E-32));
#32333=CARTESIAN_POINT('',(0.00387499999999995,-0.0085,-4.74550634669588E-19));
#32334=CARTESIAN_POINT('Origin',(-4.59950432489715E-17,-0.007,1.1450674770076E-32));
#32335=CARTESIAN_POINT('',(0.,0.,0.));
#32336=CARTESIAN_POINT('Origin',(0.02115,-0.0223,-0.01175));
#32337=CARTESIAN_POINT('',(0.02115,-0.02545,-0.00525000000000007));
#32338=CARTESIAN_POINT('',(0.02115,-0.02545,-0.00475000000000007));
#32339=CARTESIAN_POINT('',(0.0211500000000101,-0.02545000000001,-0.00849999999999003));
#32340=CARTESIAN_POINT('',(0.02115,-0.0317,-0.00475000000000007));
#32341=CARTESIAN_POINT('',(0.0211500000000101,-0.02545000000001,-0.00474999999999007));
#32342=CARTESIAN_POINT('',(0.02115,-0.0317,-0.00525000000000007));
#32343=CARTESIAN_POINT('',(0.0211500000000101,-0.0317000000000099,-0.00549999999999003));
#32344=CARTESIAN_POINT('',(0.02115000000001,-0.02545000000001,-0.00524999999999007));
#32345=CARTESIAN_POINT('Origin',(0.02115,-0.0317,0.000749999999999928));
#32346=CARTESIAN_POINT('',(0.02065,-0.0317,-0.00475000000000007));
#32347=CARTESIAN_POINT('',(0.0206500000000101,-0.03170000000001,-0.00474999999999007));
#32348=CARTESIAN_POINT('',(0.02065,-0.0317,-0.00525000000000007));
#32349=CARTESIAN_POINT('',(0.0206500000000101,-0.03170000000001,-0.00474999999999007));
#32350=CARTESIAN_POINT('',(0.0206500000000101,-0.03170000000001,-0.00524999999999007));
#32351=CARTESIAN_POINT('Origin',(0.02115,-0.02495,-0.00525000000000007));
#32352=CARTESIAN_POINT('',(0.02065,-0.02545,-0.00525000000000007));
#32353=CARTESIAN_POINT('',(0.0206500000000101,-0.02545000000001,-0.00524999999999007));
#32354=CARTESIAN_POINT('',(0.02115,-0.02495,-0.00525000000000007));
#32355=CARTESIAN_POINT('Origin',(0.02115000000001,-0.02545000000001,-0.00524999999999007));
#32356=CARTESIAN_POINT('',(0.0262,-0.02495,-0.00525000000000013));
#32357=CARTESIAN_POINT('',(0.0229000000000101,-0.02495000000001,-0.00524999999999007));
#32358=CARTESIAN_POINT('',(0.0262,-0.02545,-0.00525000000000013));
#32359=CARTESIAN_POINT('',(0.0262000000000101,-0.02495000000001,-0.00524999999999008));
#32360=CARTESIAN_POINT('',(0.0229000000000101,-0.02545000000001,-0.00524999999999007));
#32361=CARTESIAN_POINT('Origin',(0.02115,-0.02545,-0.00500000000000007));
#32362=CARTESIAN_POINT('',(0.02115,-0.02495,-0.00475000000000007));
#32363=CARTESIAN_POINT('',(0.0211500000000101,-0.02495000000001,-0.00474999999999007));
#32364=CARTESIAN_POINT('',(0.02065,-0.02545,-0.00475000000000007));
#32365=CARTESIAN_POINT('',(0.0206500000000101,-0.02545000000001,-0.00474999999999007));
#32366=CARTESIAN_POINT('Origin',(0.0211500000000101,-0.02545000000001,-0.00474999999999007));
#32367=CARTESIAN_POINT('Origin',(0.02115,-0.02495,-0.00475000000000007));
#32368=CARTESIAN_POINT('',(0.0206500000000101,-0.02545000000001,-0.00474999999999007));
#32369=CARTESIAN_POINT('',(0.0262,-0.02545,-0.00475000000000013));
#32370=CARTESIAN_POINT('',(0.0229000000000101,-0.02545000000001,-0.00474999999999007));
#32371=CARTESIAN_POINT('',(0.0262,-0.02495,-0.00475000000000013));
#32372=CARTESIAN_POINT('',(0.0262000000000101,-0.02545000000001,-0.00474999999999008));
#32373=CARTESIAN_POINT('',(0.0229000000000101,-0.02495000000001,-0.00474999999999007));
#32374=CARTESIAN_POINT('Origin',(0.02065,-0.02545,-0.00475000000000007));
#32375=CARTESIAN_POINT('Origin',(0.0229,-0.02545,-0.00475000000000009));
#32376=CARTESIAN_POINT('',(0.0262000000000101,-0.02545000000001,-0.00524999999999008));
#32377=CARTESIAN_POINT('Origin',(0.0229,-0.02495,-0.00525000000000009));
#32378=CARTESIAN_POINT('',(0.0262000000000101,-0.02495000000001,-0.00474999999999008));
#32379=CARTESIAN_POINT('Origin',(0.0262,-0.0252,-0.00500000000000013));
#32380=CARTESIAN_POINT('',(0.,0.,0.));
#32381=CARTESIAN_POINT('Origin',(0.0121040592752336,-0.01,0.00446113764208535));
#32382=CARTESIAN_POINT('',(0.0122678470666214,-0.01,0.00398872515347788));
#32383=CARTESIAN_POINT('',(0.0122678470666214,-0.0155,0.00398872515347788));
#32384=CARTESIAN_POINT('',(0.0122678470666291,-0.01000000000001,0.00398872515348977));
#32385=CARTESIAN_POINT('',(0.0119220873914306,-0.01,0.0049268481031072));
#32386=CARTESIAN_POINT('Origin',(0.0121040592752413,-0.01000000000001,0.00446113764209724));
#32387=CARTESIAN_POINT('',(0.0119220873914306,-0.0155,0.0049268481031072));
#32388=CARTESIAN_POINT('',(0.0119220873914382,-0.01000000000001,0.00492684810311909));
#32389=CARTESIAN_POINT('Origin',(0.0121040592752413,-0.01550000000001,0.00446113764209724));
#32390=CARTESIAN_POINT('Origin',(0.0113653930429603,-0.01,0.00610228162075688));
#32391=CARTESIAN_POINT('',(0.0115933339737932,-0.01,0.00565726147284101));
#32392=CARTESIAN_POINT('',(0.0115933339737932,-0.0155,0.00565726147284101));
#32393=CARTESIAN_POINT('',(0.0115933339738008,-0.01000000000001,0.0056572614728529));
#32394=CARTESIAN_POINT('',(0.0111203777280115,-0.01,0.00653813422822932));
#32395=CARTESIAN_POINT('Origin',(0.011365393042968,-0.01000000000001,0.00610228162076877));
#32396=CARTESIAN_POINT('',(0.0111203777280115,-0.0155,0.00653813422822932));
#32397=CARTESIAN_POINT('',(0.0111203777280192,-0.01000000000001,0.00653813422824121));
#32398=CARTESIAN_POINT('Origin',(0.011365393042968,-0.01550000000001,0.00610228162076877));
#32399=CARTESIAN_POINT('Origin',(0.0104055123630489,-0.01,0.00762465162892286));
#32400=CARTESIAN_POINT('',(0.0106931698223871,-0.01,0.00721568563267485));
#32401=CARTESIAN_POINT('',(0.0106931698223871,-0.0155,0.00721568563267485));
#32402=CARTESIAN_POINT('',(0.0106931698223947,-0.01000000000001,0.00721568563268675));
#32403=CARTESIAN_POINT('',(0.010102222561359,-0.01,0.00802216300761643));
#32404=CARTESIAN_POINT('Origin',(0.0104055123630566,-0.01000000000001,0.00762465162893475));
#32405=CARTESIAN_POINT('',(0.010102222561359,-0.0155,0.00802216300761643));
#32406=CARTESIAN_POINT('',(0.0101022225613666,-0.01000000000001,0.00802216300762832));
#32407=CARTESIAN_POINT('Origin',(0.0104055123630566,-0.01550000000001,0.00762465162893475));
#32408=CARTESIAN_POINT('Origin',(0.00924310022108555,-0.01,0.00899861646604452));
#32409=CARTESIAN_POINT('',(0.00958487528368847,-0.01,0.00863366467938941));
#32410=CARTESIAN_POINT('',(0.00958487528368847,-0.0155,0.00863366467938941));
#32411=CARTESIAN_POINT('',(0.00958487528369612,-0.01000000000001,0.00863366467940131));
#32412=CARTESIAN_POINT('',(0.00888743912365737,-0.01,0.00935004950913547));
#32413=CARTESIAN_POINT('Origin',(0.00924310022109321,-0.01000000000001,
0.00899861646605642));
#32414=CARTESIAN_POINT('',(0.00888743912365737,-0.0155,0.00935004950913547));
#32415=CARTESIAN_POINT('',(0.00888743912366502,-0.01000000000001,0.00935004950914736));
#32416=CARTESIAN_POINT('Origin',(0.00924310022109321,-0.01550000000001,
0.00899861646605642));
#32417=CARTESIAN_POINT('Origin',(0.00790078164718944,-0.01,0.0101974334694291));
#32418=CARTESIAN_POINT('',(0.00829002205022697,-0.01,0.00988359926376768));
#32419=CARTESIAN_POINT('',(0.00829002205022697,-0.0155,0.00988359926376768));
#32420=CARTESIAN_POINT('',(0.00829002205023463,-0.01000000000001,0.00988359926377957));
#32421=CARTESIAN_POINT('',(0.0074996717927259,-0.01,0.0104959479324828));
#32422=CARTESIAN_POINT('Origin',(0.0079007816471971,-0.01000000000001,0.010197433469441));
#32423=CARTESIAN_POINT('',(0.0074996717927259,-0.0155,0.0104959479324828));
#32424=CARTESIAN_POINT('',(0.00749967179273355,-0.01000000000001,0.0104959479324947));
#32425=CARTESIAN_POINT('Origin',(0.0079007816471971,-0.01550000000001,0.010197433469441));
#32426=CARTESIAN_POINT('Origin',(0.00640468334553672,-0.01,0.01119776902974));
#32427=CARTESIAN_POINT('',(0.00683381296731816,-0.01,0.0109411608309043));
#32428=CARTESIAN_POINT('',(0.00683381296731816,-0.0155,0.0109411608309043));
#32429=CARTESIAN_POINT('',(0.00683381296732582,-0.01000000000001,0.0109411608309161));
#32430=CARTESIAN_POINT('',(0.00596593188109928,-0.01,0.0114375546682883));
#32431=CARTESIAN_POINT('Origin',(0.00640468334554438,-0.01000000000001,
0.0111977690297519));
#32432=CARTESIAN_POINT('',(0.00596593188109928,-0.0155,0.0114375546682883));
#32433=CARTESIAN_POINT('',(0.00596593188110694,-0.01000000000001,0.0114375546683002));
#32434=CARTESIAN_POINT('Origin',(0.00640468334554438,-0.01550000000001,
0.0111977690297519));
#32435=CARTESIAN_POINT('Origin',(0.00478392516778247,-0.01,0.0119801527531604));
#32436=CARTESIAN_POINT('',(0.0052445914883475,-0.01,0.0117857651478533));
#32437=CARTESIAN_POINT('',(0.0052445914883475,-0.0155,0.0117857651478533));
#32438=CARTESIAN_POINT('',(0.00524459148835515,-0.01000000000001,0.0117857651478652));
#32439=CARTESIAN_POINT('',(0.004316071891554,-0.01,0.0121565424125011));
#32440=CARTESIAN_POINT('Origin',(0.00478392516779012,-0.01000000000001,
0.0119801527531723));
#32441=CARTESIAN_POINT('',(0.004316071891554,-0.0155,0.0121565424125011));
#32442=CARTESIAN_POINT('',(0.00431607189156165,-0.01000000000001,0.012156542412513));
#32443=CARTESIAN_POINT('Origin',(0.00478392516779012,-0.01550000000001,
0.0119801527531723));
#32444=CARTESIAN_POINT('Origin',(0.00307005332827152,-0.01,0.0125293564304624));
#32445=CARTESIAN_POINT('',(0.00355329000169056,-0.01,0.0124009729523085));
#32446=CARTESIAN_POINT('',(0.00355329000169056,-0.0155,0.0124009729523085));
#32447=CARTESIAN_POINT('',(0.00355329000169822,-0.01000000000001,0.0124009729523203));
#32448=CARTESIAN_POINT('',(0.00258220447209863,-0.01,0.0126389168865166));
#32449=CARTESIAN_POINT('Origin',(0.00307005332827917,-0.01000000000001,
0.0125293564304743));
#32450=CARTESIAN_POINT('',(0.00258220447209862,-0.0155,0.0126389168865166));
#32451=CARTESIAN_POINT('',(0.00258220447210627,-0.01000000000001,0.0126389168865285));
#32452=CARTESIAN_POINT('Origin',(0.00307005332827917,-0.01550000000001,
0.0125293564304743));
#32453=CARTESIAN_POINT('Origin',(0.00129642639285968,-0.01,0.0128346904367771));
#32454=CARTESIAN_POINT('',(0.00179282776695818,-0.01,0.0127748099241446));
#32455=CARTESIAN_POINT('',(0.00179282776695818,-0.0155,0.0127748099241446));
#32456=CARTESIAN_POINT('',(0.00179282776696584,-0.01000000000001,0.0127748099241565));
#32457=CARTESIAN_POINT('',(0.000798077379807918,-0.01,0.0128752892198909));
#32458=CARTESIAN_POINT('Origin',(0.00129642639286733,-0.01000000000001,
0.012834690436789));
#32459=CARTESIAN_POINT('',(0.000798077379807918,-0.0155,0.0128752892198909));
#32460=CARTESIAN_POINT('',(0.000798077379815572,-0.01000000000001,0.0128752892199028));
#32461=CARTESIAN_POINT('Origin',(0.00129642639286733,-0.01550000000001,
0.012834690436789));
#32462=CARTESIAN_POINT('Origin',(-0.000502434007626007,-0.01,0.0128902117929839));
#32463=CARTESIAN_POINT('',(-2.52982094668758E-6,-0.01,0.0128999997519382));
#32464=CARTESIAN_POINT('',(-2.52982094668715E-6,-0.0155,0.0128999997519382));
#32465=CARTESIAN_POINT('',(-2.52982093903355E-6,-0.01000000000001,0.0128999997519501));
#32466=CARTESIAN_POINT('',(-0.00100158338088122,-0.01,0.0128610586940245));
#32467=CARTESIAN_POINT('Origin',(-0.000502434007618353,-0.01000000000001,
0.0128902117929958));
#32468=CARTESIAN_POINT('',(-0.00100158338088122,-0.0155,0.0128610586940245));
#32469=CARTESIAN_POINT('',(-0.00100158338087356,-0.01000000000001,0.0128610586940364));
#32470=CARTESIAN_POINT('Origin',(-0.000502434007618352,-0.01550000000001,
0.0128902117929958));
#32471=CARTESIAN_POINT('Origin',(-0.00229151510166345,-0.01,0.0126948398390388));
#32472=CARTESIAN_POINT('',(-0.00179783816876445,-0.01,0.0127741057580926));
#32473=CARTESIAN_POINT('',(-0.00179783816876445,-0.0155,0.0127741057580926));
#32474=CARTESIAN_POINT('',(-0.0017978381687568,-0.01000000000001,0.0127741057581045));
#32475=CARTESIAN_POINT('',(-0.00278174946034568,-0.01,0.0125965022899163));
#32476=CARTESIAN_POINT('Origin',(-0.00229151510165579,-0.01000000000001,
0.0126948398390507));
#32477=CARTESIAN_POINT('',(-0.00278174946034568,-0.0155,0.0125965022899163));
#32478=CARTESIAN_POINT('',(-0.00278174946035758,-0.01000000000001,0.012596502289924));
#32479=CARTESIAN_POINT('Origin',(-0.00229151510165579,-0.01550000000001,
0.0126948398390507));
#32480=CARTESIAN_POINT('Origin',(-0.00403599446080683,-0.01,0.0122523772677932));
#32481=CARTESIAN_POINT('',(-0.00355815364163782,-0.01,0.0123995783259956));
#32482=CARTESIAN_POINT('',(-0.00355815364163782,-0.0155,0.0123995783259956));
#32483=CARTESIAN_POINT('',(-0.00355815364164971,-0.01000000000001,0.0123995783260032));
#32484=CARTESIAN_POINT('',(-0.00450777195075764,-0.01,0.0120867692970439));
#32485=CARTESIAN_POINT('Origin',(-0.00403599446081873,-0.01000000000001,
0.0122523772678009));
#32486=CARTESIAN_POINT('',(-0.00450777195075764,-0.0155,0.0120867692970439));
#32487=CARTESIAN_POINT('',(-0.00450777195076953,-0.01000000000001,0.0120867692970515));
#32488=CARTESIAN_POINT('Origin',(-0.00403599446081873,-0.01550000000001,
0.0122523772678009));
#32489=CARTESIAN_POINT('Origin',(-0.00570191777864627,-0.01,0.0115714361099027));
#32490=CARTESIAN_POINT('',(-0.0052492137012165,-0.01,0.0117837072060944));
#32491=CARTESIAN_POINT('',(-0.0052492137012165,-0.0155,0.0117837072060944));
#32492=CARTESIAN_POINT('',(-0.00524921370122839,-0.01000000000001,0.0117837072061021));
#32493=CARTESIAN_POINT('',(-0.0061460557876627,-0.01,0.0113417810883008));
#32494=CARTESIAN_POINT('Origin',(-0.00570191777865816,-0.01000000000001,
0.0115714361099103));
#32495=CARTESIAN_POINT('',(-0.0061460557876627,-0.0155,0.0113417810883008));
#32496=CARTESIAN_POINT('',(-0.00614605578767459,-0.01000000000001,0.0113417810883085));
#32497=CARTESIAN_POINT('Origin',(-0.00570191777865816,-0.01550000000001,
0.0115714361099103));
#32498=CARTESIAN_POINT('Origin',(-0.0072568597527597,-0.01,0.0106652701104462));
#32499=CARTESIAN_POINT('',(-0.0068381037869931,-0.01,0.0109384796291949));
#32500=CARTESIAN_POINT('',(-0.0068381037869931,-0.0155,0.0109384796291949));
#32501=CARTESIAN_POINT('',(-0.00683810378700499,-0.01000000000001,0.0109384796292026));
#32502=CARTESIAN_POINT('',(-0.00766471363969576,-0.01,0.0103760380117588));
#32503=CARTESIAN_POINT('Origin',(-0.00725685975277159,-0.01000000000001,
0.0106652701104539));
#32504=CARTESIAN_POINT('',(-0.00766471363969575,-0.0155,0.0103760380117588));
#32505=CARTESIAN_POINT('',(-0.00766471363970765,-0.01000000000001,0.0103760380117664));
#32506=CARTESIAN_POINT('Origin',(-0.00725685975277159,-0.01550000000001,
0.0106652701104539));
#32507=CARTESIAN_POINT('Origin',(-0.00867055520634127,-0.01,0.00955151675985495));
#32508=CARTESIAN_POINT('',(-0.00829389796078364,-0.01,0.00988034698864926));
#32509=CARTESIAN_POINT('',(-0.00829389796078364,-0.0155,0.00988034698864926));
#32510=CARTESIAN_POINT('',(-0.00829389796079552,-0.01000000000001,0.00988034698865692));
#32511=CARTESIAN_POINT('',(-0.00903418655921466,-0.01,0.00920833715788611));
#32512=CARTESIAN_POINT('Origin',(-0.00867055520635317,-0.01000000000001,
0.0095515167598626));
#32513=CARTESIAN_POINT('',(-0.00903418655921466,-0.0155,0.00920833715788611));
#32514=CARTESIAN_POINT('',(-0.00903418655922655,-0.01000000000001,0.00920833715789376));
#32515=CARTESIAN_POINT('Origin',(-0.00867055520635317,-0.01550000000001,
0.0095515167598626));
#32516=CARTESIAN_POINT('Origin',(-0.00991548816544177,-0.01,0.0082518540002223));
#32517=CARTESIAN_POINT('',(-0.00958826084493661,-0.01,0.0086299046326977));
#32518=CARTESIAN_POINT('',(-0.00958826084493661,-0.0155,0.0086299046326977));
#32519=CARTESIAN_POINT('',(-0.0095882608449485,-0.01000000000001,0.00862990463270536));
#32520=CARTESIAN_POINT('',(-0.0102278193135934,-0.01,0.00786140649556347));
#32521=CARTESIAN_POINT('Origin',(-0.00991548816545366,-0.01000000000001,
0.00825185400022996));
#32522=CARTESIAN_POINT('',(-0.0102278193135934,-0.0155,0.00786140649556347));
#32523=CARTESIAN_POINT('',(-0.0102278193136052,-0.01000000000001,0.00786140649557113));
#32524=CARTESIAN_POINT('Origin',(-0.00991548816545366,-0.01550000000001,
0.00825185400022996));
#32525=CARTESIAN_POINT('Origin',(-0.0109674274261026,-0.01,0.0067915782888202));
#32526=CARTESIAN_POINT('',(-0.010695999138228,-0.01,0.00721149099944164));
#32527=CARTESIAN_POINT('',(-0.010695999138228,-0.0155,0.00721149099944164));
#32528=CARTESIAN_POINT('',(-0.0106959991382398,-0.01000000000001,0.0072114909994493));
#32529=CARTESIAN_POINT('',(-0.011222379199005,-0.01,0.00636146249802205));
#32530=CARTESIAN_POINT('Origin',(-0.0109674274261145,-0.01000000000001,
0.00679157828882786));
#32531=CARTESIAN_POINT('',(-0.011222379199005,-0.0155,0.00636146249802205));
#32532=CARTESIAN_POINT('',(-0.0112223791990169,-0.01000000000001,0.00636146249802971));
#32533=CARTESIAN_POINT('Origin',(-0.0109674274261145,-0.01550000000001,
0.00679157828882786));
#32534=CARTESIAN_POINT('Origin',(-0.0118058981871781,-0.01,0.005199112231332));
#32535=CARTESIAN_POINT('',(-0.0115955519748124,-0.01,0.00565271389683093));
#32536=CARTESIAN_POINT('',(-0.0115955519748124,-0.0155,0.00565271389683093));
#32537=CARTESIAN_POINT('',(-0.0115955519748243,-0.01000000000001,0.00565271389683857));
#32538=CARTESIAN_POINT('',(-0.0119985082385752,-0.01,0.00473769986901296));
#32539=CARTESIAN_POINT('Origin',(-0.01180589818719,-0.01000000000001,0.00519911223133965));
#32540=CARTESIAN_POINT('',(-0.0119985082385752,-0.0155,0.00473769986901296));
#32541=CARTESIAN_POINT('',(-0.0119985082385871,-0.01000000000001,0.00473769986902062));
#32542=CARTESIAN_POINT('Origin',(-0.01180589818719,-0.01550000000001,0.00519911223133965));
#32543=CARTESIAN_POINT('Origin',(-0.0124145805690504,-0.01,0.00350545136816342));
#32544=CARTESIAN_POINT('',(-0.012269410581952,-0.01,0.00398391314808515));
#32545=CARTESIAN_POINT('',(-0.012269410581952,-0.0155,0.00398391314808515));
#32546=CARTESIAN_POINT('',(-0.0122694105819639,-0.01000000000001,0.00398391314809281));
#32547=CARTESIAN_POINT('',(-0.0125410999633822,-0.01,0.00302172330110727));
#32548=CARTESIAN_POINT('Origin',(-0.0124145805690623,-0.01000000000001,
0.00350545136817107));
#32549=CARTESIAN_POINT('',(-0.0125410999633822,-0.0155,0.00302172330110727));
#32550=CARTESIAN_POINT('',(-0.0125410999633941,-0.01000000000001,0.00302172330111493));
#32551=CARTESIAN_POINT('Origin',(-0.0124145805690623,-0.01550000000001,
0.00350545136817107));
#32552=CARTESIAN_POINT('Origin',(-0.0127816272615221,-0.01,0.0017435608815054));
#32553=CARTESIAN_POINT('',(-0.0127044590683616,-0.01,0.00223757006154593));
#32554=CARTESIAN_POINT('',(-0.0127044590683616,-0.0155,0.00223757006154593));
#32555=CARTESIAN_POINT('',(-0.0127044590683735,-0.01000000000001,0.00223757006155359));
#32556=CARTESIAN_POINT('',(-0.0128395934426919,-0.01,0.00124693232630483));
#32557=CARTESIAN_POINT('Origin',(-0.012781627261534,-0.01000000000001,0.00174356088151305));
#32558=CARTESIAN_POINT('',(-0.0128395934426919,-0.0155,0.00124693232630483));
#32559=CARTESIAN_POINT('',(-0.0128395934427038,-0.01000000000001,0.00124693232631249));
#32560=CARTESIAN_POINT('Origin',(-0.012781627261534,-0.01550000000001,0.00174356088151305));
#32561=CARTESIAN_POINT('Origin',(-0.0128998941182339,-0.01,-5.22660344400411E-5));
#32562=CARTESIAN_POINT('',(-0.0128922297101135,-0.01,0.00044767521895696));
#32563=CARTESIAN_POINT('',(-0.0128922297101135,-0.0155,0.00044767521895696));
#32564=CARTESIAN_POINT('',(-0.0128922297101254,-0.01000000000001,0.000447675218964614));
#32565=CARTESIAN_POINT('',(-0.0128881788404607,-0.01,-0.000552128767864633));
#32566=CARTESIAN_POINT('Origin',(-0.0128998941182458,-0.01000000000001,
-5.22660344323867E-5));
#32567=CARTESIAN_POINT('',(-0.0128881788404607,-0.0155,-0.000552128767864633));
#32568=CARTESIAN_POINT('',(-0.0128881788404726,-0.01000000000001,-0.000552128767856978));
#32569=CARTESIAN_POINT('Origin',(-0.0128998941182458,-0.01550000000001,
-5.22660344323867E-5));
#32570=CARTESIAN_POINT('Origin',(-0.0127670792093463,-0.01,-0.00184707565147683));
#32571=CARTESIAN_POINT('',(-0.012829067765252,-0.01,-0.001350933112546));
#32572=CARTESIAN_POINT('',(-0.012829067765252,-0.0155,-0.001350933112546));
#32573=CARTESIAN_POINT('',(-0.0128290677652638,-0.01000000000001,-0.00135093311253835));
#32574=CARTESIAN_POINT('',(-0.012685910497186,-0.01,-0.00234044330360477));
#32575=CARTESIAN_POINT('Origin',(-0.0127670792093582,-0.01000000000001,
-0.00184707565146918));
#32576=CARTESIAN_POINT('',(-0.012685910497186,-0.0155,-0.00234044330360477));
#32577=CARTESIAN_POINT('',(-0.0126859104971979,-0.01000000000001,-0.00234044330359712));
#32578=CARTESIAN_POINT('Origin',(-0.0127670792093582,-0.01550000000001,
-0.00184707565146918));
#32579=CARTESIAN_POINT('Origin',(-0.0123857676259861,-0.01,-0.00360593404197504));
#32580=CARTESIAN_POINT('',(-0.0125162026091882,-0.01,-0.00312324706767692));
#32581=CARTESIAN_POINT('',(-0.0125162026091882,-0.0155,-0.00312324706767692));
#32582=CARTESIAN_POINT('',(-0.0125162026091958,-0.01000000000001,-0.00312324706768881));
#32583=CARTESIAN_POINT('',(-0.0122367253360928,-0.01,-0.00408320377265504));
#32584=CARTESIAN_POINT('Origin',(-0.0123857676259938,-0.01000000000001,
-0.00360593404198693));
#32585=CARTESIAN_POINT('',(-0.0122367253360928,-0.0155,-0.00408320377265504));
#32586=CARTESIAN_POINT('',(-0.0122367253361005,-0.01000000000001,-0.00408320377266693));
#32587=CARTESIAN_POINT('Origin',(-0.0123857676259938,-0.01550000000001,
-0.00360593404198693));
#32588=CARTESIAN_POINT('Origin',(-0.011763381164388,-0.01,-0.00529460702803539));
#32589=CARTESIAN_POINT('',(-0.011959723806306,-0.01,-0.00483477057127637));
#32590=CARTESIAN_POINT('',(-0.011959723806306,-0.0155,-0.00483477057127637));
#32591=CARTESIAN_POINT('',(-0.0119597238063136,-0.01000000000001,-0.00483477057128826));
#32592=CARTESIAN_POINT('',(-0.0115493662354015,-0.01,-0.00574648932484605));
#32593=CARTESIAN_POINT('Origin',(-0.0117633811643957,-0.01000000000001,
-0.00529460702804728));
#32594=CARTESIAN_POINT('',(-0.0115493662354015,-0.0155,-0.00574648932484605));
#32595=CARTESIAN_POINT('',(-0.0115493662354091,-0.01000000000001,-0.00574648932485794));
#32596=CARTESIAN_POINT('Origin',(-0.0117633811643957,-0.01550000000001,
-0.00529460702804728));
#32597=CARTESIAN_POINT('Origin',(-0.0109120338690729,-0.01,-0.00688022651082125));
#32598=CARTESIAN_POINT('',(-0.0111704625835182,-0.01,-0.00645219076517593));
#32599=CARTESIAN_POINT('',(-0.0111704625835182,-0.0155,-0.00645219076517593));
#32600=CARTESIAN_POINT('',(-0.0111704625835258,-0.01000000000001,-0.00645219076518782));
#32601=CARTESIAN_POINT('',(-0.0106372118581474,-0.01,-0.00729792599886364));
#32602=CARTESIAN_POINT('Origin',(-0.0109120338690805,-0.01000000000001,
-0.00688022651083314));
#32603=CARTESIAN_POINT('',(-0.0106372118581474,-0.0155,-0.00729792599886364));
#32604=CARTESIAN_POINT('',(-0.010637211858155,-0.01000000000001,-0.00729792599887552));
#32605=CARTESIAN_POINT('Origin',(-0.0109120338690805,-0.01550000000001,
-0.00688022651083314));
#32606=CARTESIAN_POINT('Origin',(-0.0098482962467508,-0.01,-0.00833193021071565));
#32607=CARTESIAN_POINT('',(-0.0101637810127551,-0.01,-0.00794402640508956));
#32608=CARTESIAN_POINT('',(-0.0101637810127551,-0.0155,-0.00794402640508956));
#32609=CARTESIAN_POINT('',(-0.0101637810127627,-0.01000000000001,-0.00794402640510145));
#32610=CARTESIAN_POINT('',(-0.0095180162517236,-0.01,-0.00870731684458113));
#32611=CARTESIAN_POINT('Origin',(-0.00984829624675845,-0.01000000000001,
-0.00833193021072754));
#32612=CARTESIAN_POINT('',(-0.0095180162517236,-0.0155,-0.00870731684458113));
#32613=CARTESIAN_POINT('',(-0.00951801625173126,-0.01000000000001,-0.00870731684459302));
#32614=CARTESIAN_POINT('Origin',(-0.00984829624675845,-0.01550000000001,
-0.00833193021072754));
#32615=CARTESIAN_POINT('Origin',(-0.00859287274025656,-0.01,-0.00962146236648858));
#32616=CARTESIAN_POINT('',(-0.0089592730057083,-0.01,-0.00928124060722424));
#32617=CARTESIAN_POINT('',(-0.0089592730057083,-0.0155,-0.00928124060722424));
#32618=CARTESIAN_POINT('',(-0.00895927300571595,-0.01000000000001,-0.00928124060723613));
#32619=CARTESIAN_POINT('',(-0.00821356328554307,-0.01,-0.00994722967234497));
#32620=CARTESIAN_POINT('Origin',(-0.00859287274026421,-0.01000000000001,
-0.00962146236650047));
#32621=CARTESIAN_POINT('',(-0.00821356328554307,-0.0155,-0.00994722967234497));
#32622=CARTESIAN_POINT('',(-0.00821356328555072,-0.01000000000001,-0.00994722967235687));
#32623=CARTESIAN_POINT('Origin',(-0.00859287274026421,-0.01550000000001,
-0.00962146236650047));
#32624=CARTESIAN_POINT('Origin',(-0.00717019874012118,-0.01,-0.0107237237015491));
#32625=CARTESIAN_POINT('',(-0.00758038294062734,-0.01,-0.010437806018194));
#32626=CARTESIAN_POINT('',(-0.00758038294062734,-0.0155,-0.010437806018194));
#32627=CARTESIAN_POINT('',(-0.00758038294063499,-0.01000000000001,-0.0104378060182059));
#32628=CARTESIAN_POINT('',(-0.00674924265279915,-0.01,-0.0109935309893427));
#32629=CARTESIAN_POINT('Origin',(-0.00717019874012884,-0.01000000000001,
-0.010723723701561));
#32630=CARTESIAN_POINT('',(-0.00674924265279915,-0.0155,-0.0109935309893427));
#32631=CARTESIAN_POINT('',(-0.00674924265280681,-0.01000000000001,-0.0109935309893545));
#32632=CARTESIAN_POINT('Origin',(-0.00717019874012884,-0.01550000000001,
-0.010723723701561));
#32633=CARTESIAN_POINT('Origin',(-0.00560796497748951,-0.01,-0.0116172599528138));
#32634=CARTESIAN_POINT('',(-0.00605394934416488,-0.01,-0.011391211407848));
#32635=CARTESIAN_POINT('',(-0.00605394934416488,-0.0155,-0.011391211407848));
#32636=CARTESIAN_POINT('',(-0.00605394934417253,-0.01000000000001,-0.0113912114078599));
#32637=CARTESIAN_POINT('',(-0.00515355568896825,-0.01,-0.011825855730589));
#32638=CARTESIAN_POINT('Origin',(-0.00560796497749716,-0.01000000000001,
-0.0116172599528257));
#32639=CARTESIAN_POINT('',(-0.00515355568896825,-0.0155,-0.011825855730589));
#32640=CARTESIAN_POINT('',(-0.0051535556889759,-0.01000000000001,-0.0118258557306009));
#32641=CARTESIAN_POINT('Origin',(-0.00560796497749716,-0.01550000000001,
-0.0116172599528257));
#32642=CARTESIAN_POINT('Origin',(-0.00393657855553661,-0.01,-0.0122846794535344));
#32643=CARTESIAN_POINT('',(-0.00440968250998357,-0.01,-0.0121228998247591));
#32644=CARTESIAN_POINT('',(-0.00440968250998357,-0.0155,-0.0121228998247591));
#32645=CARTESIAN_POINT('',(-0.00440968250999122,-0.01000000000001,-0.012122899824771));
#32646=CARTESIAN_POINT('',(-0.0034575606257343,-0.01,-0.0124280036417509));
#32647=CARTESIAN_POINT('Origin',(-0.00393657855554426,-0.01000000000001,
-0.0122846794535463));
#32648=CARTESIAN_POINT('',(-0.00345756062573429,-0.0155,-0.0124280036417509));
#32649=CARTESIAN_POINT('',(-0.00345756062574195,-0.01000000000001,-0.0124280036417628));
#32650=CARTESIAN_POINT('Origin',(-0.00393657855554426,-0.01550000000001,
-0.0122846794535463));
#32651=CARTESIAN_POINT('Origin',(-0.00218857110979193,-0.01,-0.0127129916423077));
#32652=CARTESIAN_POINT('',(-0.00267958622168495,-0.01,-0.0126186297861756));
#32653=CARTESIAN_POINT('',(-0.00267958622168495,-0.0155,-0.0126186297861756));
#32654=CARTESIAN_POINT('',(-0.0026795862216926,-0.01000000000001,-0.0126186297861875));
#32655=CARTESIAN_POINT('',(-0.00169426807783735,-0.01,-0.0127882545986707));
#32656=CARTESIAN_POINT('Origin',(-0.00218857110979959,-0.01000000000001,
-0.0127129916423196));
#32657=CARTESIAN_POINT('',(-0.00169426807783735,-0.0155,-0.0127882545986707));
#32658=CARTESIAN_POINT('',(-0.00169426807784501,-0.01000000000001,-0.0127882545986826));
#32659=CARTESIAN_POINT('Origin',(-0.00218857110979959,-0.01550000000001,
-0.0127129916423196));
#32660=CARTESIAN_POINT('Origin',(-0.000397965616857901,-0.01,-0.0128938599095771));
#32661=CARTESIAN_POINT('',(-0.000897334835565383,-0.01,-0.0128687524722826));
#32662=CARTESIAN_POINT('',(-0.000897334835565383,-0.0155,-0.0128687524722826));
#32663=CARTESIAN_POINT('',(-0.000897334835573037,-0.01000000000001,-0.0128687524722945));
#32664=CARTESIAN_POINT('',(0.000102001470993323,-0.01,-0.0128995967262514));
#32665=CARTESIAN_POINT('Origin',(-0.000397965616865556,-0.01000000000001,
-0.012893859909589));
#32666=CARTESIAN_POINT('',(0.000102001470993324,-0.0155,-0.0128995967262514));
#32667=CARTESIAN_POINT('',(0.000102001470985668,-0.01000000000001,-0.0128995967262633));
#32668=CARTESIAN_POINT('Origin',(-0.000397965616865556,-0.01550000000001,
-0.012893859909589));
#32669=CARTESIAN_POINT('Origin',(0.00140038582412907,-0.01,-0.0128237638602548));
#32670=CARTESIAN_POINT('',(0.000902382152425213,-0.01,-0.0128683995295057));
#32671=CARTESIAN_POINT('',(0.000902382152425214,-0.0155,-0.0128683995295057));
#32672=CARTESIAN_POINT('',(0.000902382152417559,-0.01000000000001,-0.0128683995295176));
#32673=CARTESIAN_POINT('',(0.00189628567721606,-0.01,-0.0127598628766294));
#32674=CARTESIAN_POINT('Origin',(0.00140038582412142,-0.01000000000001,
-0.0128237638602667));
#32675=CARTESIAN_POINT('',(0.00189628567721606,-0.0155,-0.0127598628766294));
#32676=CARTESIAN_POINT('',(0.0018962856772084,-0.01000000000001,-0.0127598628766413));
#32677=CARTESIAN_POINT('Origin',(0.00140038582412142,-0.01550000000001,
-0.0128237638602667));
#32678=CARTESIAN_POINT('Origin',(0.00317148034796465,-0.01,-0.0125040678342079));
#32679=CARTESIAN_POINT('',(0.00268453529826336,-0.01,-0.0126175778274746));
#32680=CARTESIAN_POINT('',(0.00268453529826336,-0.0155,-0.0126175778274746));
#32681=CARTESIAN_POINT('',(0.0026845352982557,-0.01000000000001,-0.0126175778274865));
#32682=CARTESIAN_POINT('',(0.0036536608397248,-0.01,-0.0123717728102428));
#32683=CARTESIAN_POINT('Origin',(0.00317148034797655,-0.01000000000001,
-0.0125040678342156));
#32684=CARTESIAN_POINT('',(0.0036536608397248,-0.0155,-0.0123717728102428));
#32685=CARTESIAN_POINT('',(0.00365366083973669,-0.01000000000001,-0.0123717728102504));
#32686=CARTESIAN_POINT('Origin',(0.00317148034797655,-0.01550000000001,
-0.0125040678342156));
#32687=CARTESIAN_POINT('Origin',(0.00488084561433254,-0.01,-0.0119409943509345));
#32688=CARTESIAN_POINT('',(0.00441443701813444,-0.01,-0.0121211693253137));
#32689=CARTESIAN_POINT('',(0.00441443701813444,-0.0155,-0.0121211693253137));
#32690=CARTESIAN_POINT('',(0.00441443701814632,-0.01000000000001,-0.0121211693253213));
#32691=CARTESIAN_POINT('',(0.00533992164996587,-0.01,-0.0117428802587877));
#32692=CARTESIAN_POINT('Origin',(0.00488084561434443,-0.01000000000001,
-0.0119409943509422));
#32693=CARTESIAN_POINT('',(0.00533992164996587,-0.0155,-0.0117428802587877));
#32694=CARTESIAN_POINT('',(0.00533992164997777,-0.01000000000001,-0.0117428802587953));
#32695=CARTESIAN_POINT('Origin',(0.00488084561434443,-0.01550000000001,
-0.0119409943509422));
#32696=CARTESIAN_POINT('Origin',(0.00649521077269703,-0.01,-0.0111455029953));
#32697=CARTESIAN_POINT('',(0.00605841674279519,-0.01,-0.0113888360498612));
#32698=CARTESIAN_POINT('',(0.00605841674279519,-0.0155,-0.0113888360498612));
#32699=CARTESIAN_POINT('',(0.00605841674280708,-0.01000000000001,-0.0113888360498688));
#32700=CARTESIAN_POINT('',(0.00692224695936122,-0.01,-0.0108854259004236));
#32701=CARTESIAN_POINT('Origin',(0.00649521077270892,-0.01000000000001,
-0.0111455029953076));
#32702=CARTESIAN_POINT('',(0.00692224695936122,-0.0155,-0.0108854259004236));
#32703=CARTESIAN_POINT('',(0.00692224695937311,-0.01000000000001,-0.0108854259004312));
#32704=CARTESIAN_POINT('Origin',(0.00649521077270892,-0.01550000000001,
-0.0111455029953076));
#32705=CARTESIAN_POINT('Origin',(0.00798315404156373,-0.01,-0.0101330771016836));
#32706=CARTESIAN_POINT('',(0.00758447627690437,-0.01,-0.0104348320353073));
#32707=CARTESIAN_POINT('',(0.00758447627690437,-0.0155,-0.0104348320353073));
#32708=CARTESIAN_POINT('',(0.00758447627691625,-0.01000000000001,-0.0104348320353149));
#32709=CARTESIAN_POINT('',(0.00836983860563182,-0.01,-0.0098160991088963));
#32710=CARTESIAN_POINT('Origin',(0.00798315404157562,-0.01000000000001,
-0.0101330771016913));
#32711=CARTESIAN_POINT('',(0.00836983860563182,-0.0155,-0.0098160991088963));
#32712=CARTESIAN_POINT('',(0.00836983860564371,-0.01000000000001,-0.00981609910890396));
#32713=CARTESIAN_POINT('Origin',(0.00798315404157562,-0.01550000000001,
-0.0101330771016913));
#32714=CARTESIAN_POINT('Origin',(0.00931571429771449,-0.01,-0.00892342238848729));
#32715=CARTESIAN_POINT('',(0.00896291260749749,-0.01,-0.00927772588463158));
#32716=CARTESIAN_POINT('',(0.00896291260749749,-0.0155,-0.00927772588463158));
#32717=CARTESIAN_POINT('',(0.00896291260750937,-0.01000000000001,-0.00927772588463924));
#32718=CARTESIAN_POINT('',(0.00965452086399409,-0.01,-0.00855571311386156));
#32719=CARTESIAN_POINT('Origin',(0.00931571429772638,-0.01000000000001,
-0.00892342238849495));
#32720=CARTESIAN_POINT('',(0.00965452086399409,-0.0155,-0.00855571311386156));
#32721=CARTESIAN_POINT('',(0.00965452086400598,-0.01000000000001,-0.00855571311386922));
#32722=CARTESIAN_POINT('Origin',(0.00931571429772638,-0.01550000000001,
-0.00892342238849495));
#32723=CARTESIAN_POINT('Origin',(0.0104669547715282,-0.01,-0.00754008340874168));
#32724=CARTESIAN_POINT('',(0.0101668960393476,-0.01,-0.00794003935286826));
#32725=CARTESIAN_POINT('',(0.0101668960393476,-0.0155,-0.00794003935286826));
#32726=CARTESIAN_POINT('',(0.0101668960393595,-0.01000000000001,-0.00794003935287591));
#32727=CARTESIAN_POINT('',(0.0107512888555934,-0.01,-0.00712879989504486));
#32728=CARTESIAN_POINT('Origin',(0.0104669547715401,-0.01000000000001,-0.00754008340874933));
#32729=CARTESIAN_POINT('',(0.0107512888555934,-0.0155,-0.00712879989504486));
#32730=CARTESIAN_POINT('',(0.0107512888556053,-0.01000000000001,-0.00712879989505252));
#32731=CARTESIAN_POINT('Origin',(0.0104669547715401,-0.01550000000001,-0.00754008340874933));
#32732=CARTESIAN_POINT('Origin',(0.0114144678766987,-0.01,-0.00600998528216265));
#32733=CARTESIAN_POINT('',(0.0111729924044647,-0.01,-0.00644780898676229));
#32734=CARTESIAN_POINT('',(0.0111729924044647,-0.0155,-0.00644780898676229));
#32735=CARTESIAN_POINT('',(0.0111729924044766,-0.01000000000001,-0.00644780898676994));
#32736=CARTESIAN_POINT('',(0.0116387952390284,-0.01,-0.00556313269516086));
#32737=CARTESIAN_POINT('Origin',(0.0114144678767106,-0.01000000000001,-0.0060099852821703));
#32738=CARTESIAN_POINT('',(0.0116387952390284,-0.0155,-0.00556313269516086));
#32739=CARTESIAN_POINT('',(0.0116387952390403,-0.01000000000001,-0.00556313269516851));
#32740=CARTESIAN_POINT('Origin',(0.0114144678767106,-0.01550000000001,-0.0060099852821703));
#32741=CARTESIAN_POINT('Origin',(0.0121398113484141,-0.01,-0.00436290962832323));
#32742=CARTESIAN_POINT('',(0.0119616191815194,-0.01,-0.004830079353003));
#32743=CARTESIAN_POINT('',(0.0119616191815194,-0.0155,-0.004830079353003));
#32744=CARTESIAN_POINT('',(0.0119616191815313,-0.01000000000001,-0.00483007935301066));
#32745=CARTESIAN_POINT('',(0.0122997657120691,-0.01,-0.00388918544533519));
#32746=CARTESIAN_POINT('Origin',(0.012139811348426,-0.01000000000001,-0.00436290962833088));
#32747=CARTESIAN_POINT('',(0.0122997657120691,-0.0155,-0.00388918544533519));
#32748=CARTESIAN_POINT('',(0.012299765712081,-0.01000000000001,-0.00388918544534284));
#32749=CARTESIAN_POINT('Origin',(0.012139811348426,-0.01550000000001,-0.00436290962833088));
#32750=CARTESIAN_POINT('Origin',(0.0126288672010633,-0.01,-0.00263091490130466));
#32751=CARTESIAN_POINT('',(0.012517426647346,-0.01,-0.00311833771877137));
#32752=CARTESIAN_POINT('',(0.012517426647346,-0.0155,-0.00311833771877137));
#32753=CARTESIAN_POINT('',(0.0125174266473579,-0.01000000000001,-0.00311833771877902));
#32754=CARTESIAN_POINT('',(0.0127213352363006,-0.01,-0.00213953962469893));
#32755=CARTESIAN_POINT('Origin',(0.0126288672010752,-0.01000000000001,-0.00263091490131231));
#32756=CARTESIAN_POINT('',(0.0127213352363006,-0.0155,-0.00213953962469893));
#32757=CARTESIAN_POINT('',(0.0127213352363125,-0.01000000000001,-0.00213953962470658));
#32758=CARTESIAN_POINT('Origin',(0.0126288672010752,-0.01550000000001,-0.00263091490131231));
#32759=CARTESIAN_POINT('Origin',(0.0128721165187673,-0.01,-0.000847712408353549));
#32760=CARTESIAN_POINT('',(0.0128295966418437,-0.01,-0.00134590118790042));
#32761=CARTESIAN_POINT('',(0.0128295966418437,-0.0155,-0.00134590118790042));
#32762=CARTESIAN_POINT('',(0.0128295966418555,-0.01000000000001,-0.00134590118790808));
#32763=CARTESIAN_POINT('',(0.0128952984404617,-0.01,-0.000348250098958184));
#32764=CARTESIAN_POINT('Origin',(0.0128721165187792,-0.01000000000001,-0.000847712408361203));
#32765=CARTESIAN_POINT('',(0.0128952984404617,-0.0155,-0.000348250098958184));
#32766=CARTESIAN_POINT('',(0.0128952984404736,-0.01000000000001,-0.000348250098965837));
#32767=CARTESIAN_POINT('Origin',(0.0128721165187792,-0.01550000000001,-0.000847712408361203));
#32768=CARTESIAN_POINT('Origin',(0.0128648247302491,-0.01,0.000951989842367618));
#32769=CARTESIAN_POINT('',(0.0128920531311578,-0.01,0.000452731778653103));
#32770=CARTESIAN_POINT('',(0.0128920531311578,-0.0155,0.000452731778653103));
#32771=CARTESIAN_POINT('',(0.0128920531311697,-0.01000000000001,0.000452731778645449));
#32772=CARTESIAN_POINT('',(0.0128182693286638,-0.01,0.00144981771883018));
#32773=CARTESIAN_POINT('Origin',(0.012864824730261,-0.01000000000001,0.000951989842359964));
#32774=CARTESIAN_POINT('',(0.0128182693286638,-0.0155,0.00144981771883019));
#32775=CARTESIAN_POINT('',(0.0128182693286757,-0.01000000000001,0.00144981771882252));
#32776=CARTESIAN_POINT('Origin',(0.012864824730261,-0.01550000000001,0.000951989842359964));
#32777=CARTESIAN_POINT('Origin',(-4.47228396786959E-17,-0.01,1.11925812962326E-32));
#32778=CARTESIAN_POINT('',(0.0124917471849488,-0.01,0.00321966648386474));
#32779=CARTESIAN_POINT('Origin',(-4.47228396786953E-17,-0.01000000000001,
1.11925812962343E-32));
#32780=CARTESIAN_POINT('',(0.0127035804707671,-0.01,0.00224255283610991));
#32781=CARTESIAN_POINT('Origin',(0.0126071337618875,-0.01000000000001,0.00273316269368159));
#32782=CARTESIAN_POINT('Origin',(-4.47228396786953E-17,-0.01000000000001,
1.11925812962343E-32));
#32783=CARTESIAN_POINT('Origin',(-4.47228396786953E-17,-0.01000000000001,
1.11925812962343E-32));
#32784=CARTESIAN_POINT('Origin',(-4.47228396786953E-17,-0.01000000000001,
1.11925812962343E-32));
#32785=CARTESIAN_POINT('Origin',(-4.47228396786953E-17,-0.01000000000001,
1.11925812962343E-32));
#32786=CARTESIAN_POINT('Origin',(-4.47228396786953E-17,-0.01000000000001,
1.11925812962343E-32));
#32787=CARTESIAN_POINT('Origin',(-4.47228396786953E-17,-0.01000000000001,
1.11925812962343E-32));
#32788=CARTESIAN_POINT('Origin',(-4.47228396786953E-17,-0.01000000000001,
1.11925812962343E-32));
#32789=CARTESIAN_POINT('Origin',(-4.47228396786953E-17,-0.01000000000001,
1.11925812962343E-32));
#32790=CARTESIAN_POINT('Origin',(-4.47228396786953E-17,-0.01000000000001,
1.11925812962343E-32));
#32791=CARTESIAN_POINT('Origin',(-4.47228396786953E-17,-0.01000000000001,
1.11925812962343E-32));
#32792=CARTESIAN_POINT('Origin',(-4.47228396786953E-17,-0.01000000000001,
1.11925812962343E-32));
#32793=CARTESIAN_POINT('Origin',(-4.47228396786953E-17,-0.01000000000001,
1.11925812962343E-32));
#32794=CARTESIAN_POINT('Origin',(-4.47228396786953E-17,-0.01000000000001,
1.11925812962343E-32));
#32795=CARTESIAN_POINT('Origin',(-4.47228396786953E-17,-0.01000000000001,
1.11925812962343E-32));
#32796=CARTESIAN_POINT('Origin',(-4.47228396786953E-17,-0.01000000000001,
1.11925812962343E-32));
#32797=CARTESIAN_POINT('Origin',(-4.47228396786953E-17,-0.01000000000001,
1.11925812962343E-32));
#32798=CARTESIAN_POINT('Origin',(-4.47228396786953E-17,-0.01000000000001,
1.11925812962343E-32));
#32799=CARTESIAN_POINT('Origin',(-4.47228396786953E-17,-0.01000000000001,
1.11925812962343E-32));
#32800=CARTESIAN_POINT('Origin',(-4.47228396786953E-17,-0.01000000000001,
1.11925812962343E-32));
#32801=CARTESIAN_POINT('Origin',(-4.47228396786953E-17,-0.01000000000001,
1.11925812962343E-32));
#32802=CARTESIAN_POINT('Origin',(-4.47228396786953E-17,-0.01000000000001,
1.11925812962343E-32));
#32803=CARTESIAN_POINT('Origin',(-4.47228396786953E-17,-0.01000000000001,
1.11925812962343E-32));
#32804=CARTESIAN_POINT('Origin',(-4.47228396786953E-17,-0.01000000000001,
1.11925812962343E-32));
#32805=CARTESIAN_POINT('Origin',(-4.47228396786953E-17,-0.01000000000001,
1.11925812962343E-32));
#32806=CARTESIAN_POINT('Origin',(-4.47228396786953E-17,-0.01000000000001,
1.11925812962343E-32));
#32807=CARTESIAN_POINT('Origin',(-4.47228396786953E-17,-0.01000000000001,
1.11925812962343E-32));
#32808=CARTESIAN_POINT('Origin',(-4.47228396786953E-17,-0.01000000000001,
1.11925812962343E-32));
#32809=CARTESIAN_POINT('Origin',(-4.47228396786953E-17,-0.01000000000001,
1.11925812962343E-32));
#32810=CARTESIAN_POINT('Origin',(-4.47228396786953E-17,-0.01000000000001,
1.11925812962343E-32));
#32811=CARTESIAN_POINT('Origin',(-4.47228396786953E-17,-0.01000000000001,
1.11925812962343E-32));
#32812=CARTESIAN_POINT('Origin',(-4.47228396786953E-17,-0.01000000000001,
1.11925812962343E-32));
#32813=CARTESIAN_POINT('Origin',(-4.47228396786953E-17,-0.01000000000001,
1.11925812962343E-32));
#32814=CARTESIAN_POINT('Origin',(-4.47228396786953E-17,-0.01000000000001,
1.11925812962343E-32));
#32815=CARTESIAN_POINT('Origin',(-4.47228396786953E-17,-0.01000000000001,
1.11925812962343E-32));
#32816=CARTESIAN_POINT('Origin',(-4.47228396786953E-17,-0.01000000000001,
1.11925812962343E-32));
#32817=CARTESIAN_POINT('Origin',(-4.47228396786953E-17,-0.01000000000001,
1.11925812962343E-32));
#32818=CARTESIAN_POINT('Origin',(-4.47228396786953E-17,-0.01000000000001,
1.11925812962343E-32));
#32819=CARTESIAN_POINT('Origin',(-4.47228396786953E-17,-0.01000000000001,
1.11925812962343E-32));
#32820=CARTESIAN_POINT('Origin',(-4.47228396786953E-17,-0.01000000000001,
1.11925812962343E-32));
#32821=CARTESIAN_POINT('Origin',(-4.47228396786953E-17,-0.01000000000001,
1.11925812962343E-32));
#32822=CARTESIAN_POINT('Origin',(-4.47228396786953E-17,-0.01000000000001,
1.11925812962343E-32));
#32823=CARTESIAN_POINT('Origin',(-4.47228396786953E-17,-0.01000000000001,
1.11925812962343E-32));
#32824=CARTESIAN_POINT('Origin',(-4.47228396786953E-17,-0.01000000000001,
1.11925812962343E-32));
#32825=CARTESIAN_POINT('Origin',(-4.47228396786953E-17,-0.01000000000001,
1.11925812962343E-32));
#32826=CARTESIAN_POINT('',(-0.000529682692573584,-0.01000000000001,0.0024432429771081));
#32827=CARTESIAN_POINT('Origin',(-4.47228396786953E-17,-0.01000000000001,
1.11925812962343E-32));
#32828=CARTESIAN_POINT('Origin',(-4.43566503645872E-17,-0.0155,1.21332054810713E-32));
#32829=CARTESIAN_POINT('',(0.0124917471849488,-0.0155,0.00321966648386474));
#32830=CARTESIAN_POINT('Origin',(-4.43566503645865E-17,-0.01550000000001,
1.21332054810731E-32));
#32831=CARTESIAN_POINT('',(0.0124917471849565,-0.01000000000001,0.00321966648387663));
#32832=CARTESIAN_POINT('Origin',(-4.43566503645872E-17,-0.0155,1.21332054810713E-32));
#32833=CARTESIAN_POINT('',(0.0127035804707671,-0.0155,0.00224255283610991));
#32834=CARTESIAN_POINT('',(0.012703580470779,-0.01000000000001,0.00224255283610226));
#32835=CARTESIAN_POINT('Origin',(-4.43566503645865E-17,-0.01550000000001,
1.21332054810731E-32));
#32836=CARTESIAN_POINT('Origin',(-4.43566503645872E-17,-0.0155,1.21332054810713E-32));
#32837=CARTESIAN_POINT('Origin',(-4.43566503645865E-17,-0.01550000000001,
1.21332054810731E-32));
#32838=CARTESIAN_POINT('Origin',(-4.43566503645872E-17,-0.0155,1.21332054810713E-32));
#32839=CARTESIAN_POINT('Origin',(-4.43566503645865E-17,-0.01550000000001,
1.21332054810731E-32));
#32840=CARTESIAN_POINT('Origin',(-4.43566503645872E-17,-0.0155,1.21332054810713E-32));
#32841=CARTESIAN_POINT('Origin',(-4.43566503645865E-17,-0.01550000000001,
1.21332054810731E-32));
#32842=CARTESIAN_POINT('Origin',(-4.43566503645872E-17,-0.0155,1.21332054810713E-32));
#32843=CARTESIAN_POINT('Origin',(-4.43566503645865E-17,-0.01550000000001,
1.21332054810731E-32));
#32844=CARTESIAN_POINT('Origin',(-4.43566503645872E-17,-0.0155,1.21332054810713E-32));
#32845=CARTESIAN_POINT('Origin',(-4.43566503645865E-17,-0.01550000000001,
1.21332054810731E-32));
#32846=CARTESIAN_POINT('Origin',(-4.43566503645872E-17,-0.0155,1.21332054810713E-32));
#32847=CARTESIAN_POINT('Origin',(-4.43566503645865E-17,-0.01550000000001,
1.21332054810731E-32));
#32848=CARTESIAN_POINT('Origin',(-4.43566503645872E-17,-0.0155,1.21332054810713E-32));
#32849=CARTESIAN_POINT('Origin',(-4.43566503645865E-17,-0.01550000000001,
1.21332054810731E-32));
#32850=CARTESIAN_POINT('Origin',(-4.43566503645872E-17,-0.0155,1.21332054810713E-32));
#32851=CARTESIAN_POINT('Origin',(-4.43566503645865E-17,-0.01550000000001,
1.21332054810731E-32));
#32852=CARTESIAN_POINT('Origin',(-4.43566503645872E-17,-0.0155,1.21332054810713E-32));
#32853=CARTESIAN_POINT('Origin',(-4.43566503645865E-17,-0.01550000000001,
1.21332054810731E-32));
#32854=CARTESIAN_POINT('Origin',(-4.43566503645872E-17,-0.0155,1.21332054810713E-32));
#32855=CARTESIAN_POINT('Origin',(-4.43566503645865E-17,-0.01550000000001,
1.21332054810731E-32));
#32856=CARTESIAN_POINT('Origin',(-4.43566503645872E-17,-0.0155,1.21332054810713E-32));
#32857=CARTESIAN_POINT('Origin',(-4.43566503645865E-17,-0.01550000000001,
1.21332054810731E-32));
#32858=CARTESIAN_POINT('Origin',(-4.43566503645872E-17,-0.0155,1.21332054810713E-32));
#32859=CARTESIAN_POINT('Origin',(-4.43566503645865E-17,-0.01550000000001,
1.21332054810731E-32));
#32860=CARTESIAN_POINT('Origin',(-4.43566503645872E-17,-0.0155,1.21332054810713E-32));
#32861=CARTESIAN_POINT('Origin',(-4.43566503645865E-17,-0.01550000000001,
1.21332054810731E-32));
#32862=CARTESIAN_POINT('Origin',(-4.43566503645872E-17,-0.0155,1.21332054810713E-32));
#32863=CARTESIAN_POINT('Origin',(-4.43566503645865E-17,-0.01550000000001,
1.21332054810731E-32));
#32864=CARTESIAN_POINT('Origin',(-4.43566503645872E-17,-0.0155,1.21332054810713E-32));
#32865=CARTESIAN_POINT('Origin',(-4.43566503645865E-17,-0.01550000000001,
1.21332054810731E-32));
#32866=CARTESIAN_POINT('Origin',(-4.43566503645872E-17,-0.0155,1.21332054810713E-32));
#32867=CARTESIAN_POINT('Origin',(-4.43566503645865E-17,-0.01550000000001,
1.21332054810731E-32));
#32868=CARTESIAN_POINT('Origin',(-4.43566503645872E-17,-0.0155,1.21332054810713E-32));
#32869=CARTESIAN_POINT('Origin',(-4.43566503645865E-17,-0.01550000000001,
1.21332054810731E-32));
#32870=CARTESIAN_POINT('Origin',(-4.43566503645872E-17,-0.0155,1.21332054810713E-32));
#32871=CARTESIAN_POINT('Origin',(-4.43566503645865E-17,-0.01550000000001,
1.21332054810731E-32));
#32872=CARTESIAN_POINT('Origin',(-4.43566503645872E-17,-0.0155,1.21332054810713E-32));
#32873=CARTESIAN_POINT('Origin',(-4.43566503645865E-17,-0.01550000000001,
1.21332054810731E-32));
#32874=CARTESIAN_POINT('Origin',(-4.43566503645872E-17,-0.0155,1.21332054810713E-32));
#32875=CARTESIAN_POINT('Origin',(-4.43566503645865E-17,-0.01550000000001,
1.21332054810731E-32));
#32876=CARTESIAN_POINT('Origin',(-4.43566503645872E-17,-0.0155,1.21332054810713E-32));
#32877=CARTESIAN_POINT('Origin',(-4.43566503645865E-17,-0.01550000000001,
1.21332054810731E-32));
#32878=CARTESIAN_POINT('Origin',(-4.43566503645872E-17,-0.0155,1.21332054810713E-32));
#32879=CARTESIAN_POINT('Origin',(-4.43566503645865E-17,-0.01550000000001,
1.21332054810731E-32));
#32880=CARTESIAN_POINT('Origin',(-4.43566503645872E-17,-0.0155,1.21332054810713E-32));
#32881=CARTESIAN_POINT('Origin',(-4.43566503645865E-17,-0.01550000000001,
1.21332054810731E-32));
#32882=CARTESIAN_POINT('Origin',(-4.43566503645872E-17,-0.0155,1.21332054810713E-32));
#32883=CARTESIAN_POINT('Origin',(-4.43566503645865E-17,-0.01550000000001,
1.21332054810731E-32));
#32884=CARTESIAN_POINT('Origin',(-4.43566503645872E-17,-0.0155,1.21332054810713E-32));
#32885=CARTESIAN_POINT('Origin',(-4.43566503645865E-17,-0.01550000000001,
1.21332054810731E-32));
#32886=CARTESIAN_POINT('Origin',(-4.43566503645872E-17,-0.0155,1.21332054810713E-32));
#32887=CARTESIAN_POINT('Origin',(-4.43566503645865E-17,-0.01550000000001,
1.21332054810731E-32));
#32888=CARTESIAN_POINT('Origin',(-4.43566503645872E-17,-0.0155,1.21332054810713E-32));
#32889=CARTESIAN_POINT('Origin',(-4.43566503645865E-17,-0.01550000000001,
1.21332054810731E-32));
#32890=CARTESIAN_POINT('Origin',(-4.43566503645872E-17,-0.0155,1.21332054810713E-32));
#32891=CARTESIAN_POINT('Origin',(-4.43566503645865E-17,-0.01550000000001,
1.21332054810731E-32));
#32892=CARTESIAN_POINT('Origin',(-4.43566503645872E-17,-0.0155,1.21332054810713E-32));
#32893=CARTESIAN_POINT('Origin',(-4.43566503645865E-17,-0.01550000000001,
1.21332054810731E-32));
#32894=CARTESIAN_POINT('Origin',(-4.43566503645872E-17,-0.0155,1.21332054810713E-32));
#32895=CARTESIAN_POINT('Origin',(-4.43566503645865E-17,-0.01550000000001,
1.21332054810731E-32));
#32896=CARTESIAN_POINT('Origin',(-4.43566503645872E-17,-0.0155,1.21332054810713E-32));
#32897=CARTESIAN_POINT('Origin',(-4.43566503645865E-17,-0.01550000000001,
1.21332054810731E-32));
#32898=CARTESIAN_POINT('Origin',(-4.43566503645872E-17,-0.0155,1.21332054810713E-32));
#32899=CARTESIAN_POINT('Origin',(-4.43566503645865E-17,-0.01550000000001,
1.21332054810731E-32));
#32900=CARTESIAN_POINT('Origin',(-4.43566503645872E-17,-0.0155,1.21332054810713E-32));
#32901=CARTESIAN_POINT('Origin',(-4.43566503645865E-17,-0.01550000000001,
1.21332054810731E-32));
#32902=CARTESIAN_POINT('Origin',(-4.43566503645872E-17,-0.0155,1.21332054810713E-32));
#32903=CARTESIAN_POINT('Origin',(-4.43566503645865E-17,-0.01550000000001,
1.21332054810731E-32));
#32904=CARTESIAN_POINT('Origin',(-4.43566503645872E-17,-0.0155,1.21332054810713E-32));
#32905=CARTESIAN_POINT('Origin',(-4.43566503645865E-17,-0.01550000000001,
1.21332054810731E-32));
#32906=CARTESIAN_POINT('Origin',(-4.43566503645872E-17,-0.0155,1.21332054810713E-32));
#32907=CARTESIAN_POINT('Origin',(-4.43566503645865E-17,-0.01550000000001,
1.21332054810731E-32));
#32908=CARTESIAN_POINT('Origin',(-4.43566503645872E-17,-0.0155,1.21332054810713E-32));
#32909=CARTESIAN_POINT('Origin',(-4.43566503645865E-17,-0.01550000000001,
1.21332054810731E-32));
#32910=CARTESIAN_POINT('Origin',(-4.43566503645872E-17,-0.0155,1.21332054810713E-32));
#32911=CARTESIAN_POINT('Origin',(-4.43566503645865E-17,-0.01550000000001,
1.21332054810731E-32));
#32912=CARTESIAN_POINT('Origin',(-4.43566503645872E-17,-0.0155,1.21332054810713E-32));
#32913=CARTESIAN_POINT('Origin',(-4.43566503645865E-17,-0.01550000000001,
1.21332054810731E-32));
#32914=CARTESIAN_POINT('Origin',(-4.43566503645872E-17,-0.0155,1.21332054810713E-32));
#32915=CARTESIAN_POINT('Origin',(-4.43566503645865E-17,-0.01550000000001,
1.21332054810731E-32));
#32916=CARTESIAN_POINT('Origin',(-4.43566503645872E-17,-0.0155,1.21332054810713E-32));
#32917=CARTESIAN_POINT('Origin',(-4.43566503645865E-17,-0.01550000000001,
1.21332054810731E-32));
#32918=CARTESIAN_POINT('Origin',(-4.43566503645872E-17,-0.0155,1.21332054810713E-32));
#32919=CARTESIAN_POINT('Origin',(-4.43566503645865E-17,-0.01550000000001,
1.21332054810731E-32));
#32920=CARTESIAN_POINT('Origin',(0.0126071337618777,-0.01,0.00273316269367947));
#32921=CARTESIAN_POINT('Origin',(0.0126071337618875,-0.01550000000001,0.00273316269368159));
#32922=CARTESIAN_POINT('Origin',(-4.43566503645872E-17,-0.0155,1.21332054810713E-32));
#32923=CARTESIAN_POINT('Origin',(-4.43566503645865E-17,-0.01550000000001,
1.21332054810731E-32));
#32924=CARTESIAN_POINT('',(-0.000529682692573584,-0.01550000000001,0.0024432429771081));
#32925=CARTESIAN_POINT('Origin',(-4.43566503645865E-17,-0.01550000000001,
1.21332054810731E-32));
#32926=CARTESIAN_POINT('Origin',(-4.43566503645872E-17,-0.0155,1.21332054810713E-32));
#32927=CARTESIAN_POINT('Origin',(-4.43566503645872E-17,-0.0155,1.21332054810713E-32));
#32928=CARTESIAN_POINT('',(-0.000529682692573584,-0.0155,0.0024432429771081));
#32929=CARTESIAN_POINT('',(0.,0.,0.));
#32930=CARTESIAN_POINT('Origin',(-4.34919666873154E-17,-0.030975,7.19534755436855E-33));
#32931=CARTESIAN_POINT('',(-0.00249999999970682,-0.03097500000001,-3.89374311628611E-8));
#32932=CARTESIAN_POINT('',(-3.89374412069654E-8,-0.03097500000001,0.00249999999970677));
#32933=CARTESIAN_POINT('Origin',(-4.34919666873148E-17,-0.03097500000001,
7.19534755436887E-33));
#32934=CARTESIAN_POINT('',(-4.32205597349135E-8,-0.03125000000001,0.00277499999967342));
#32935=CARTESIAN_POINT('Origin',(-4.32205597347746E-8,-0.030975,0.00277499999966342));
#32936=CARTESIAN_POINT('Origin',(-4.34751277937011E-17,-0.03125000000001,
7.20399477813186E-33));
#32937=CARTESIAN_POINT('Origin',(-4.34919666873148E-17,-0.03097500000001,
7.19534755436887E-33));
#32938=CARTESIAN_POINT('Origin',(-4.36282086447352E-17,-0.02875,7.12538365301343E-33));
#32939=CARTESIAN_POINT('',(-0.00249999999970682,-0.02652500000001,-3.89374311628611E-8));
#32940=CARTESIAN_POINT('',(-3.89374412072379E-8,-0.02652500000001,0.00249999999970677));
#32941=CARTESIAN_POINT('Origin',(-4.37644506021545E-17,-0.02652500000001,
7.05541975165862E-33));
#32942=CARTESIAN_POINT('',(-0.00249999999969682,-0.02875,-3.89374411633177E-8));
#32943=CARTESIAN_POINT('Origin',(-4.37644506021545E-17,-0.02652500000001,
7.05541975165862E-33));
#32944=CARTESIAN_POINT('Origin',(0.00341666666625222,-0.03125,5.32145029227824E-8));
#32945=CARTESIAN_POINT('',(-0.0043333333328078,-0.03125000000001,-6.74915646830841E-8));
#32946=CARTESIAN_POINT('Origin',(-4.34751277937011E-17,-0.03125000000001,
7.20399477813186E-33));
#32947=CARTESIAN_POINT('Origin',(-4.37644506021551E-17,-0.026525,7.0554197516583E-33));
#32948=CARTESIAN_POINT('',(-4.32205597352196E-8,-0.02625000000001,0.00277499999967342));
#32949=CARTESIAN_POINT('Origin',(-4.37812894957682E-17,-0.02625000000001,
7.04677252789562E-33));
#32950=CARTESIAN_POINT('Origin',(-4.32205597350471E-8,-0.026525,0.00277499999966342));
#32951=CARTESIAN_POINT('Origin',(0.00341666666625222,-0.02625,5.32145029227824E-8));
#32952=CARTESIAN_POINT('',(-0.0043333333328078,-0.02625000000001,-6.74915646830841E-8));
#32953=CARTESIAN_POINT('Origin',(-4.37812894957682E-17,-0.02625000000001,
7.04677252789562E-33));
#32954=CARTESIAN_POINT('Origin',(-4.36282086447352E-17,-0.02875,7.12538365301343E-33));
#32955=CARTESIAN_POINT('',(-0.0043333333328078,-0.02875,-6.74915646830841E-8));
#32956=CARTESIAN_POINT('',(0.,0.,0.));
#32957=CARTESIAN_POINT('Origin',(0.0126992616256242,-0.008,0.00360121565085291));
#32958=CARTESIAN_POINT('',(0.0126265137841014,-0.008,0.00384039707060321));
#32959=CARTESIAN_POINT('',(0.0129397779442914,-0.008,0.00366942049272513));
#32960=CARTESIAN_POINT('Origin',(0.0126992616256341,-0.00799999999999,0.00360121565086291));
#32961=CARTESIAN_POINT('',(0.0129397779442914,-0.024,0.00366942049272513));
#32962=CARTESIAN_POINT('',(0.0129397779443013,-0.00799999999999,0.00366942049273513));
#32963=CARTESIAN_POINT('',(0.0126265137841014,-0.024,0.00384039707060321));
#32964=CARTESIAN_POINT('Origin',(0.0126992616256341,-0.02400000000001,0.00360121565086291));
#32965=CARTESIAN_POINT('',(0.0126265137841114,-0.00799999999999,0.00384039707061321));
#32966=CARTESIAN_POINT('Origin',(-4.44089209850063E-17,-0.008,6.72997231505748E-33));
#32967=CARTESIAN_POINT('',(0.0130408866654485,-0.008,0.0032920776082785));
#32968=CARTESIAN_POINT('Origin',(-4.44089209850063E-17,-0.00799999999999,
6.72997231505748E-33));
#32969=CARTESIAN_POINT('',(0.0130408866654485,-0.024,0.0032920776082785));
#32970=CARTESIAN_POINT('',(0.0130408866654585,-0.00799999999999,0.0032920776082885));
#32971=CARTESIAN_POINT('Origin',(-4.44089209850063E-17,-0.02400000000001,
6.72997231505748E-33));
#32972=CARTESIAN_POINT('Origin',(0.0127984910025219,-0.008,0.00323088657466738));
#32973=CARTESIAN_POINT('',(0.0128550802335678,-0.008,0.00298737546828897));
#32974=CARTESIAN_POINT('Origin',(0.0127984910025319,-0.00799999999999,0.00323088657467738));
#32975=CARTESIAN_POINT('',(0.0128550802335678,-0.024,0.00298737546828897));
#32976=CARTESIAN_POINT('',(0.0128550802335778,-0.00799999999999,0.00298737546829897));
#32977=CARTESIAN_POINT('Origin',(0.0127984910025319,-0.02400000000001,0.00323088657467738));
#32978=CARTESIAN_POINT('Origin',(0.0126625775316771,-0.008,0.00294264001438602));
#32979=CARTESIAN_POINT('',(0.0126625775316771,-0.008,0.00294264001438602));
#32980=CARTESIAN_POINT('',(0.0125348531511851,-0.00799999999999,0.00291295831081412));
#32981=CARTESIAN_POINT('',(0.0126625775316771,-0.024,0.00294264001438602));
#32982=CARTESIAN_POINT('',(0.0126625775316871,-0.016,0.00294264001439602));
#32983=CARTESIAN_POINT('',(0.0125348531511851,-0.02400000000001,0.00291295831081412));
#32984=CARTESIAN_POINT('Origin',(0.0130606706482359,-0.008,0.00191282048773811));
#32985=CARTESIAN_POINT('',(0.0130197646145518,-0.008,0.00215945117603184));
#32986=CARTESIAN_POINT('',(0.0133080318347555,-0.008,0.00194904814849073));
#32987=CARTESIAN_POINT('Origin',(0.0130606706482459,-0.00799999999999,0.00191282048774811));
#32988=CARTESIAN_POINT('',(0.0133080318347555,-0.024,0.00194904814849073));
#32989=CARTESIAN_POINT('',(0.0133080318347655,-0.00799999999999,0.00194904814850073));
#32990=CARTESIAN_POINT('',(0.0130197646145518,-0.024,0.00215945117603184));
#32991=CARTESIAN_POINT('Origin',(0.0130606706482459,-0.02400000000001,0.00191282048774811));
#32992=CARTESIAN_POINT('',(0.0130197646145618,-0.00799999999999,0.00215945117604184));
#32993=CARTESIAN_POINT('Origin',(-4.44089209850063E-17,-0.008,6.72997231505748E-33));
#32994=CARTESIAN_POINT('',(0.0133590224269186,-0.008,0.00156173614835727));
#32995=CARTESIAN_POINT('Origin',(-4.44089209850063E-17,-0.00799999999999,
6.72997231505748E-33));
#32996=CARTESIAN_POINT('',(0.0133590224269186,-0.024,0.00156173614835727));
#32997=CARTESIAN_POINT('',(0.0133590224269286,-0.00799999999999,0.00156173614836727));
#32998=CARTESIAN_POINT('Origin',(-4.44089209850063E-17,-0.02400000000001,
6.72997231505748E-33));
#32999=CARTESIAN_POINT('Origin',(0.0131107134598755,-0.008,0.00153270759541383));
#33000=CARTESIAN_POINT('',(0.0131350339847262,-0.008,0.00128389338345843));
#33001=CARTESIAN_POINT('Origin',(0.0131107134598855,-0.00799999999999,0.00153270759542383));
#33002=CARTESIAN_POINT('',(0.0131350339847262,-0.024,0.00128389338345843));
#33003=CARTESIAN_POINT('',(0.0131350339847362,-0.00799999999999,0.00128389338346843));
#33004=CARTESIAN_POINT('Origin',(0.0131107134598855,-0.02400000000001,0.00153270759542383));
#33005=CARTESIAN_POINT('Origin',(0.0129383390216809,-0.008,0.00126466729223498));
#33006=CARTESIAN_POINT('',(0.0129383390216809,-0.008,0.00126466729223498));
#33007=CARTESIAN_POINT('',(0.0129458744527519,-0.00799999999999,0.00126540384839641));
#33008=CARTESIAN_POINT('',(0.0129383390216809,-0.024,0.00126466729223498));
#33009=CARTESIAN_POINT('',(0.0129383390216909,-0.016,0.00126466729224498));
#33010=CARTESIAN_POINT('',(0.0129458744527519,-0.02400000000001,0.00126540384839641));
#33011=CARTESIAN_POINT('Origin',(0.0131986079749541,-0.008,0.00019169643574408));
#33012=CARTESIAN_POINT('',(0.0131902436626865,-0.008,0.000441556473125589));
#33013=CARTESIAN_POINT('',(0.0134485816108434,-0.008,0.000195327050057415));
#33014=CARTESIAN_POINT('Origin',(0.0131986079749641,-0.00799999999999,0.00019169643575408));
#33015=CARTESIAN_POINT('',(0.0134485816108434,-0.024,0.000195327050057415));
#33016=CARTESIAN_POINT('',(0.0134485816108534,-0.00799999999999,0.000195327050067415));
#33017=CARTESIAN_POINT('',(0.0131902436626865,-0.024,0.000441556473125589));
#33018=CARTESIAN_POINT('Origin',(0.0131986079749641,-0.02400000000001,0.00019169643575408));
#33019=CARTESIAN_POINT('',(0.0131902436626965,-0.00799999999999,0.000441556473135589));
#33020=CARTESIAN_POINT('Origin',(-4.44089209850063E-17,-0.008,6.72997231505748E-33));
#33021=CARTESIAN_POINT('',(0.0134485816108434,-0.008,-0.000195327050057413));
#33022=CARTESIAN_POINT('Origin',(-4.44089209850063E-17,-0.00799999999999,
6.72997231505748E-33));
#33023=CARTESIAN_POINT('',(0.0134485816108434,-0.024,-0.000195327050057413));
#33024=CARTESIAN_POINT('',(0.0134485816108534,-0.00799999999999,-0.000195327050067413));
#33025=CARTESIAN_POINT('Origin',(-4.44089209850063E-17,-0.02400000000001,
6.72997231505748E-33));
#33026=CARTESIAN_POINT('Origin',(0.0131986079749541,-0.008,-0.000191696435744079));
#33027=CARTESIAN_POINT('',(0.0131902436626865,-0.008,-0.000441556473125588));
#33028=CARTESIAN_POINT('Origin',(0.0131986079749641,-0.00799999999999,-0.000191696435754079));
#33029=CARTESIAN_POINT('',(0.0131902436626865,-0.024,-0.000441556473125588));
#33030=CARTESIAN_POINT('',(0.0131902436626965,-0.00799999999999,-0.000441556473135588));
#33031=CARTESIAN_POINT('Origin',(0.0131986079749641,-0.02400000000001,-0.000191696435754079));
#33032=CARTESIAN_POINT('Origin',(0.0129927219438385,-0.008,-0.000434944237918216));
#33033=CARTESIAN_POINT('',(0.0129927219438385,-0.008,-0.000434944237918216));
#33034=CARTESIAN_POINT('',(0.0130276266077339,-0.00799999999999,-0.000436112706129034));
#33035=CARTESIAN_POINT('',(0.0129927219438385,-0.024,-0.000434944237918216));
#33036=CARTESIAN_POINT('',(0.0129927219438485,-0.016,-0.000434944237928215));
#33037=CARTESIAN_POINT('',(0.0130276266077339,-0.02400000000001,-0.000436112706129034));
#33038=CARTESIAN_POINT('Origin',(0.0131107134598755,-0.008,-0.00153270759541383));
#33039=CARTESIAN_POINT('',(0.0131350339847262,-0.008,-0.00128389338345843));
#33040=CARTESIAN_POINT('',(0.0133590224269186,-0.008,-0.00156173614835727));
#33041=CARTESIAN_POINT('Origin',(0.0131107134598855,-0.00799999999999,-0.00153270759542383));
#33042=CARTESIAN_POINT('',(0.0133590224269186,-0.024,-0.00156173614835727));
#33043=CARTESIAN_POINT('',(0.0133590224269286,-0.00799999999999,-0.00156173614836727));
#33044=CARTESIAN_POINT('',(0.0131350339847262,-0.024,-0.00128389338345843));
#33045=CARTESIAN_POINT('Origin',(0.0131107134598855,-0.02400000000001,-0.00153270759542383));
#33046=CARTESIAN_POINT('',(0.0131350339847362,-0.00799999999999,-0.00128389338346843));
#33047=CARTESIAN_POINT('Origin',(-4.44089209850063E-17,-0.008,6.72997231505748E-33));
#33048=CARTESIAN_POINT('',(0.0133080318347555,-0.008,-0.00194904814849073));
#33049=CARTESIAN_POINT('Origin',(-4.44089209850063E-17,-0.00799999999999,
6.72997231505748E-33));
#33050=CARTESIAN_POINT('',(0.0133080318347555,-0.024,-0.00194904814849073));
#33051=CARTESIAN_POINT('',(0.0133080318347655,-0.00799999999999,-0.00194904814850073));
#33052=CARTESIAN_POINT('Origin',(-4.44089209850063E-17,-0.02400000000001,
6.72997231505748E-33));
#33053=CARTESIAN_POINT('Origin',(0.0130606706482359,-0.008,-0.00191282048773811));
#33054=CARTESIAN_POINT('',(0.0130197646145518,-0.008,-0.00215945117603184));
#33055=CARTESIAN_POINT('Origin',(0.0130606706482459,-0.00799999999999,-0.00191282048774811));
#33056=CARTESIAN_POINT('',(0.0130197646145518,-0.024,-0.00215945117603184));
#33057=CARTESIAN_POINT('',(0.0130197646145618,-0.00799999999999,-0.00215945117604184));
#33058=CARTESIAN_POINT('Origin',(0.0130606706482459,-0.02400000000001,-0.00191282048774811));
#33059=CARTESIAN_POINT('Origin',(0.0128247957912738,-0.008,-0.00212711375157131));
#33060=CARTESIAN_POINT('',(0.0128247957912738,-0.008,-0.00212711375157131));
#33061=CARTESIAN_POINT('',(0.0127759261415696,-0.00799999999999,-0.00211900825769013));
#33062=CARTESIAN_POINT('',(0.0128247957912738,-0.024,-0.00212711375157131));
#33063=CARTESIAN_POINT('',(0.0128247957912839,-0.016,-0.00212711375158131));
#33064=CARTESIAN_POINT('',(0.0127759261415696,-0.02400000000001,-0.00211900825769013));
#33065=CARTESIAN_POINT('Origin',(0.0127984910025219,-0.008,-0.00323088657466738));
#33066=CARTESIAN_POINT('',(0.0128550802335678,-0.008,-0.00298737546828897));
#33067=CARTESIAN_POINT('',(0.0130408866654485,-0.008,-0.0032920776082785));
#33068=CARTESIAN_POINT('Origin',(0.0127984910025319,-0.00799999999999,-0.00323088657467738));
#33069=CARTESIAN_POINT('',(0.0130408866654485,-0.024,-0.0032920776082785));
#33070=CARTESIAN_POINT('',(0.0130408866654585,-0.00799999999999,-0.0032920776082885));
#33071=CARTESIAN_POINT('',(0.0128550802335678,-0.024,-0.00298737546828897));
#33072=CARTESIAN_POINT('Origin',(0.0127984910025319,-0.02400000000001,-0.00323088657467738));
#33073=CARTESIAN_POINT('',(0.0128550802335778,-0.00799999999999,-0.00298737546829897));
#33074=CARTESIAN_POINT('Origin',(-4.44089209850063E-17,-0.008,6.72997231505748E-33));
#33075=CARTESIAN_POINT('',(0.0129397779442914,-0.008,-0.00366942049272513));
#33076=CARTESIAN_POINT('Origin',(-4.44089209850063E-17,-0.00799999999999,
6.72997231505748E-33));
#33077=CARTESIAN_POINT('',(0.0129397779442914,-0.024,-0.00366942049272513));
#33078=CARTESIAN_POINT('',(0.0129397779443013,-0.00799999999999,-0.00366942049273513));
#33079=CARTESIAN_POINT('Origin',(-4.44089209850063E-17,-0.02400000000001,
6.72997231505748E-33));
#33080=CARTESIAN_POINT('Origin',(0.0126992616256242,-0.008,-0.00360121565085291));
#33081=CARTESIAN_POINT('',(0.0126265137841014,-0.008,-0.00384039707060321));
#33082=CARTESIAN_POINT('Origin',(0.0126992616256341,-0.00799999999999,-0.00360121565086291));
#33083=CARTESIAN_POINT('',(0.0126265137841014,-0.024,-0.00384039707060321));
#33084=CARTESIAN_POINT('',(0.0126265137841114,-0.00799999999999,-0.00384039707061321));
#33085=CARTESIAN_POINT('Origin',(0.0126992616256341,-0.02400000000001,-0.00360121565086291));
#33086=CARTESIAN_POINT('Origin',(0.0124374338270155,-0.008,-0.00378288775918766));
#33087=CARTESIAN_POINT('',(0.0124374338270155,-0.008,-0.00378288775918766));
#33088=CARTESIAN_POINT('',(0.0122036407116943,-0.00799999999999,-0.00371177878877263));
#33089=CARTESIAN_POINT('',(0.0124374338270155,-0.024,-0.00378288775918766));
#33090=CARTESIAN_POINT('',(0.0124374338270255,-0.016,-0.00378288775919766));
#33091=CARTESIAN_POINT('',(0.0122036407116943,-0.02400000000001,-0.00371177878877263));
#33092=CARTESIAN_POINT('Origin',(0.0131008975231583,-0.008,-0.00304450063026861));
#33093=CARTESIAN_POINT('',(0.0126625775316771,-0.024,-0.00294264001438602));
#33094=CARTESIAN_POINT('',(0.0127540131469256,-0.02400000000001,-0.00296388861875541));
#33095=CARTESIAN_POINT('',(0.0126625775316771,-0.008,-0.00294264001438602));
#33096=CARTESIAN_POINT('',(0.0126625775316871,-0.016,-0.00294264001439602));
#33097=CARTESIAN_POINT('',(0.0127540131469256,-0.00799999999999,-0.00296388861875541));
#33098=CARTESIAN_POINT('Origin',(0.0133862046032006,-0.008,-0.00130844423696619));
#33099=CARTESIAN_POINT('',(0.0129383390216809,-0.024,-0.00126466729223498));
#33100=CARTESIAN_POINT('',(0.0131698072435117,-0.02400000000001,-0.00128729232076201));
#33101=CARTESIAN_POINT('',(0.0129383390216809,-0.008,-0.00126466729223498));
#33102=CARTESIAN_POINT('',(0.0129383390216909,-0.016,-0.00126466729224498));
#33103=CARTESIAN_POINT('',(0.0131698072435117,-0.00799999999999,-0.00128729232076201));
#33104=CARTESIAN_POINT('Origin',(0.0132687310302026,-0.008,0.00220074461220262));
#33105=CARTESIAN_POINT('',(0.0128247957912738,-0.024,0.00212711375157131));
#33106=CARTESIAN_POINT('',(0.0129978937610339,-0.02400000000001,0.00215582368800579));
#33107=CARTESIAN_POINT('',(0.0128247957912738,-0.008,0.00212711375157131));
#33108=CARTESIAN_POINT('',(0.0128247957912839,-0.016,0.0021271137515813));
#33109=CARTESIAN_POINT('',(0.0129978937610339,-0.00799999999999,0.00215582368800579));
#33110=CARTESIAN_POINT('Origin',(0.012867960382566,-0.008,0.00391383387392877));
#33111=CARTESIAN_POINT('',(0.0124374338270155,-0.024,0.00378288775918766));
#33112=CARTESIAN_POINT('',(0.0124189039894696,-0.02400000000001,0.00377725184614318));
#33113=CARTESIAN_POINT('',(0.0124374338270155,-0.008,0.00378288775918766));
#33114=CARTESIAN_POINT('',(0.0124374338270255,-0.016,0.00378288775919766));
#33115=CARTESIAN_POINT('',(0.0124189039894696,-0.00799999999999,0.00377725184614318));
#33116=CARTESIAN_POINT('Origin',(-4.44089209850063E-17,-0.016,6.72997231505748E-33));
#33117=CARTESIAN_POINT('',(0.0122543393841983,-0.008,-0.00433948917003902));
#33118=CARTESIAN_POINT('Origin',(-4.44089209850063E-17,-0.00799999999999,
6.72997231505748E-33));
#33119=CARTESIAN_POINT('',(0.0122543393841983,-0.024,-0.00433948917003902));
#33120=CARTESIAN_POINT('',(0.0122543393842083,-0.016,-0.00433948917004902));
#33121=CARTESIAN_POINT('Origin',(-4.44089209850063E-17,-0.02400000000001,
6.72997231505748E-33));
#33122=CARTESIAN_POINT('Origin',(-4.44089209850063E-17,-0.016,6.72997231505748E-33));
#33123=CARTESIAN_POINT('Origin',(-4.44089209850063E-17,-0.02400000000001,
6.72997231505748E-33));
#33124=CARTESIAN_POINT('Origin',(-4.44089209850063E-17,-0.00799999999999,
6.72997231505748E-33));
#33125=CARTESIAN_POINT('Origin',(0.0130771696920991,-0.024,1.11022302462517E-18));
#33126=CARTESIAN_POINT('',(0.0131027167261813,-0.024,-0.00463991534334942));
#33127=CARTESIAN_POINT('',(0.0131027167261912,-0.02400000000001,-0.00463991534335942));
#33128=CARTESIAN_POINT('',(0.0131027167261813,-0.024,0.00463991534334942));
#33129=CARTESIAN_POINT('Origin',(-4.44089209850063E-17,-0.02400000000001,
6.72997231505748E-33));
#33130=CARTESIAN_POINT('',(0.0122543393841983,-0.024,0.00433948917003903));
#33131=CARTESIAN_POINT('',(0.0122543393842083,-0.02400000000001,0.00433948917004903));
#33132=CARTESIAN_POINT('Origin',(-4.44089209850063E-17,-0.02400000000001,
6.72997231505748E-33));
#33133=CARTESIAN_POINT('Origin',(-4.44089209850063E-17,-0.02400000000001,
6.72997231505748E-33));
#33134=CARTESIAN_POINT('',(0.0129927219438385,-0.024,0.000434944237918216));
#33135=CARTESIAN_POINT('Origin',(-4.44089209850063E-17,-0.02400000000001,
6.72997231505748E-33));
#33136=CARTESIAN_POINT('',(0.0132525006413773,-0.02400000000001,0.000443640587169928));
#33137=CARTESIAN_POINT('Origin',(-4.44089209850063E-17,-0.02400000000001,
6.72997231505748E-33));
#33138=CARTESIAN_POINT('Origin',(-4.44089209850063E-17,-0.016,6.72997231505748E-33));
#33139=CARTESIAN_POINT('',(0.0129927219438385,-0.008,0.000434944237918216));
#33140=CARTESIAN_POINT('Origin',(-4.44089209850063E-17,-0.00799999999999,
6.72997231505748E-33));
#33141=CARTESIAN_POINT('',(0.0129927219438485,-0.016,0.000434944237928217));
#33142=CARTESIAN_POINT('Origin',(-4.44089209850063E-17,-0.016,6.72997231505748E-33));
#33143=CARTESIAN_POINT('',(0.0122543393841983,-0.008,0.00433948917003903));
#33144=CARTESIAN_POINT('',(0.0122543393842083,-0.016,0.00433948917004903));
#33145=CARTESIAN_POINT('Origin',(-4.44089209850063E-17,-0.00799999999999,
6.72997231505748E-33));
#33146=CARTESIAN_POINT('Origin',(0.0134424700111252,-0.008,0.00045));
#33147=CARTESIAN_POINT('',(0.0132525006413773,-0.00799999999999,0.000443640587169928));
#33148=CARTESIAN_POINT('Origin',(-4.44089209850063E-17,-0.016,6.72997231505748E-33));
#33149=CARTESIAN_POINT('Origin',(-4.44089209850063E-17,-0.00799999999999,
6.72997231505748E-33));
#33150=CARTESIAN_POINT('Origin',(0.0131027167261813,-0.016,-0.00463991534334942));
#33151=CARTESIAN_POINT('',(0.0131027167261813,-0.008,-0.00463991534334942));
#33152=CARTESIAN_POINT('',(0.0131027167261912,-0.00799999999999,-0.00463991534335942));
#33153=CARTESIAN_POINT('',(0.0131027167261912,-0.016,-0.00463991534335942));
#33154=CARTESIAN_POINT('Origin',(-4.44089209850063E-17,-0.016,6.72997231505748E-33));
#33155=CARTESIAN_POINT('',(0.0131027167261813,-0.008,0.00463991534334942));
#33156=CARTESIAN_POINT('Origin',(-4.44089209850063E-17,-0.00799999999999,
6.72997231505748E-33));
#33157=CARTESIAN_POINT('',(0.0131027167261912,-0.016,0.00463991534335942));
#33158=CARTESIAN_POINT('Origin',(0.0122543393841983,-0.016,0.00433948917003903));
#33159=CARTESIAN_POINT('',(0.0122543393842083,-0.00799999999999,0.00433948917004903));
#33160=CARTESIAN_POINT('Origin',(-4.44089209850063E-17,-0.016,6.72997231505748E-33));
#33161=CARTESIAN_POINT('Origin',(-4.44089209850063E-17,-0.00799999999999,
6.72997231505748E-33));
#33162=CARTESIAN_POINT('Origin',(0.0130771696920991,-0.008,1.11022302462517E-18));
#33163=CARTESIAN_POINT('',(0.,0.,0.));
#33164=CARTESIAN_POINT('Origin',(0.02115,-0.0223,-0.01175));
#33165=CARTESIAN_POINT('',(0.02115,-0.02545,0.000749999999999928));
#33166=CARTESIAN_POINT('',(0.02115,-0.02545,0.00124999999999993));
#33167=CARTESIAN_POINT('',(0.02115000000001,-0.02545000000001,-0.00549999999999003));
#33168=CARTESIAN_POINT('',(0.02115,-0.0317,0.00124999999999993));
#33169=CARTESIAN_POINT('',(0.02115000000001,-0.02545000000001,0.00125000000000993));
#33170=CARTESIAN_POINT('',(0.02115,-0.0317,0.000749999999999928));
#33171=CARTESIAN_POINT('',(0.0211500000000101,-0.0317000000000099,-0.00549999999999003));
#33172=CARTESIAN_POINT('',(0.0211500000000101,-0.02545000000001,0.000750000000009929));
#33173=CARTESIAN_POINT('Origin',(0.02065,-0.02545,0.00124999999999993));
#33174=CARTESIAN_POINT('',(0.02065,-0.02545,0.000749999999999933));
#33175=CARTESIAN_POINT('',(0.02065,-0.02545,0.00124999999999993));
#33176=CARTESIAN_POINT('',(0.0206500000000101,-0.02545000000001,0.00125000000000993));
#33177=CARTESIAN_POINT('',(0.02065,-0.0317,0.000749999999999933));
#33178=CARTESIAN_POINT('',(0.0206500000000101,-0.02545000000001,0.000750000000009934));
#33179=CARTESIAN_POINT('',(0.02065,-0.0317,0.00124999999999993));
#33180=CARTESIAN_POINT('',(0.0206500000000101,-0.03170000000001,0.00125000000000993));
#33181=CARTESIAN_POINT('',(0.0206500000000101,-0.02545000000001,0.00125000000000993));
#33182=CARTESIAN_POINT('Origin',(0.02115,-0.0317,0.000749999999999928));
#33183=CARTESIAN_POINT('',(0.0206500000000101,-0.03170000000001,0.00125000000000993));
#33184=CARTESIAN_POINT('',(0.0206500000000101,-0.03170000000001,0.000750000000009934));
#33185=CARTESIAN_POINT('Origin',(0.02115,-0.02495,0.00124999999999993));
#33186=CARTESIAN_POINT('',(0.02115,-0.02495,0.00124999999999993));
#33187=CARTESIAN_POINT('Origin',(0.02115000000001,-0.02545000000001,0.00125000000000993));
#33188=CARTESIAN_POINT('',(0.0262,-0.02545,0.00124999999999987));
#33189=CARTESIAN_POINT('',(0.0229000000000101,-0.02545000000001,0.00125000000000991));
#33190=CARTESIAN_POINT('',(0.0262,-0.02495,0.00124999999999987));
#33191=CARTESIAN_POINT('',(0.0262000000000101,-0.02545000000001,0.00125000000000997));
#33192=CARTESIAN_POINT('',(0.0229000000000101,-0.02495000000001,0.00125000000000991));
#33193=CARTESIAN_POINT('Origin',(0.02115,-0.02545,0.000999999999999926));
#33194=CARTESIAN_POINT('',(0.02115,-0.02495,0.000749999999999928));
#33195=CARTESIAN_POINT('',(0.0211500000000101,-0.02495000000001,0.00125000000000993));
#33196=CARTESIAN_POINT('Origin',(0.0211500000000101,-0.02545000000001,0.000750000000009929));
#33197=CARTESIAN_POINT('Origin',(0.02115,-0.02495,0.000749999999999928));
#33198=CARTESIAN_POINT('',(0.0262,-0.02495,0.000749999999999874));
#33199=CARTESIAN_POINT('',(0.0229000000000101,-0.02495000000001,0.000750000000009909));
#33200=CARTESIAN_POINT('',(0.0262,-0.02545,0.000749999999999874));
#33201=CARTESIAN_POINT('',(0.0262000000000101,-0.02495000000001,0.000750000000009974));
#33202=CARTESIAN_POINT('',(0.0229000000000101,-0.02545000000001,0.000750000000009909));
#33203=CARTESIAN_POINT('Origin',(0.0229,-0.02545,0.00124999999999991));
#33204=CARTESIAN_POINT('',(0.0262000000000101,-0.02545000000001,0.000750000000009974));
#33205=CARTESIAN_POINT('Origin',(0.0229,-0.02495,0.000749999999999909));
#33206=CARTESIAN_POINT('',(0.0262000000000101,-0.02495000000001,0.00125000000000997));
#33207=CARTESIAN_POINT('Origin',(0.0262,-0.0252,0.000999999999999873));
#33208=CARTESIAN_POINT('',(0.,0.,0.));
#33209=CARTESIAN_POINT('Origin',(-0.0129631448730622,-0.016,-0.01915));
#33210=CARTESIAN_POINT('',(-0.0129631448730622,-0.008,-0.02115));
#33211=CARTESIAN_POINT('',(-0.0129631448730622,-0.024,-0.02115));
#33212=CARTESIAN_POINT('',(-0.0129631448730622,-0.008,-0.02115));
#33213=CARTESIAN_POINT('',(-0.0140842817269487,-0.024,-0.0208062162162162));
#33214=CARTESIAN_POINT('Origin',(-0.0129631448730722,-0.02400000000001,
-0.0191500000000101));
#33215=CARTESIAN_POINT('',(-0.0140842817269487,-0.008,-0.0208062162162162));
#33216=CARTESIAN_POINT('',(-0.0140842817269635,-0.008,-0.0208062162162381));
#33217=CARTESIAN_POINT('Origin',(-0.0129631448730722,-0.00799999999999,
-0.0191500000000101));
#33218=CARTESIAN_POINT('Origin',(0.0135625633639073,-0.016,-0.02115));
#33219=CARTESIAN_POINT('',(0.0129631448730622,-0.008,-0.02115));
#33220=CARTESIAN_POINT('',(0.0129631448730622,-0.024,-0.02115));
#33221=CARTESIAN_POINT('',(0.0129631448730622,-0.008,-0.0211500000000226));
#33222=CARTESIAN_POINT('',(0.0135625633639173,-0.02400000000001,-0.02115000000001));
#33223=CARTESIAN_POINT('',(0.0135625633639173,-0.00799999999999,-0.02115000000001));
#33224=CARTESIAN_POINT('Origin',(0.0129631448730622,-0.016,-0.01915));
#33225=CARTESIAN_POINT('',(0.0140842817269487,-0.008,-0.0208062162162162));
#33226=CARTESIAN_POINT('',(0.0140842817269487,-0.024,-0.0208062162162162));
#33227=CARTESIAN_POINT('',(0.0140842817269487,-0.008,-0.0208062162162162));
#33228=CARTESIAN_POINT('Origin',(0.0129631448730722,-0.02400000000001,-0.0191500000000101));
#33229=CARTESIAN_POINT('Origin',(0.0129631448730722,-0.00799999999999,-0.0191500000000101));
#33230=CARTESIAN_POINT('Origin',(-2.55351295663785E-17,-0.016,-3.88578058618804E-17));
#33231=CARTESIAN_POINT('',(0.0208062162162162,-0.008,-0.0140842817269487));
#33232=CARTESIAN_POINT('',(0.0208062162162162,-0.024,-0.0140842817269487));
#33233=CARTESIAN_POINT('',(0.020806216216238,-0.008,-0.0140842817269635));
#33234=CARTESIAN_POINT('Origin',(-1.00255351295664E-14,-0.02400000000001,
9.96114219413812E-15));
#33235=CARTESIAN_POINT('Origin',(-1.00255351295664E-14,-0.00799999999999,
9.96114219413812E-15));
#33236=CARTESIAN_POINT('Origin',(0.01915,-0.016,-0.0129631448730622));
#33237=CARTESIAN_POINT('',(0.02115,-0.008,-0.0129631448730622));
#33238=CARTESIAN_POINT('',(0.02115,-0.024,-0.0129631448730622));
#33239=CARTESIAN_POINT('',(0.02115,-0.008,-0.0129631448730622));
#33240=CARTESIAN_POINT('Origin',(0.01915000000001,-0.02400000000001,-0.0129631448730722));
#33241=CARTESIAN_POINT('Origin',(0.01915000000001,-0.00799999999999,-0.0129631448730722));
#33242=CARTESIAN_POINT('Origin',(0.02115,-0.016,0.0135625633639073));
#33243=CARTESIAN_POINT('',(0.02115,-0.008,0.0129631448730622));
#33244=CARTESIAN_POINT('',(0.02115,-0.024,0.0129631448730622));
#33245=CARTESIAN_POINT('',(0.0211500000000225,-0.008,0.0129631448730622));
#33246=CARTESIAN_POINT('',(0.02115000000001,-0.02400000000001,0.0135625633639173));
#33247=CARTESIAN_POINT('',(0.02115000000001,-0.00799999999999,0.0135625633639173));
#33248=CARTESIAN_POINT('Origin',(0.01915,-0.016,0.0129631448730622));
#33249=CARTESIAN_POINT('',(0.0208062162162162,-0.008,0.0140842817269487));
#33250=CARTESIAN_POINT('',(0.0208062162162162,-0.024,0.0140842817269487));
#33251=CARTESIAN_POINT('',(0.0208062162162262,-0.016,0.0140842817269587));
#33252=CARTESIAN_POINT('Origin',(0.01915000000001,-0.02400000000001,0.0129631448730722));
#33253=CARTESIAN_POINT('Origin',(0.01915000000001,-0.00799999999999,0.0129631448730722));
#33254=CARTESIAN_POINT('Origin',(-2.55351295663785E-17,-0.016,-3.88578058618804E-17));
#33255=CARTESIAN_POINT('',(0.0140842817269487,-0.024,0.0208062162162161));
#33256=CARTESIAN_POINT('',(0.0140842817269487,-0.008,0.0208062162162161));
#33257=CARTESIAN_POINT('',(0.0140842817269587,-0.016,0.0208062162162262));
#33258=CARTESIAN_POINT('Origin',(-1.00255351295664E-14,-0.02400000000001,
9.96114219413812E-15));
#33259=CARTESIAN_POINT('Origin',(-1.00255351295664E-14,-0.00799999999999,
9.96114219413812E-15));
#33260=CARTESIAN_POINT('Origin',(-0.01915,-0.016,-0.0129631448730623));
#33261=CARTESIAN_POINT('',(-0.0208062162162162,-0.008,-0.0140842817269487));
#33262=CARTESIAN_POINT('',(-0.0208062162162162,-0.024,-0.0140842817269487));
#33263=CARTESIAN_POINT('',(-0.0208062162162425,-0.008,-0.0140842817269665));
#33264=CARTESIAN_POINT('',(-0.02115,-0.024,-0.0129631448730623));
#33265=CARTESIAN_POINT('Origin',(-0.01915000000001,-0.02400000000001,-0.0129631448730723));
#33266=CARTESIAN_POINT('',(-0.02115,-0.008,-0.0129631448730623));
#33267=CARTESIAN_POINT('',(-0.0211500000000225,-0.008,-0.0129631448730623));
#33268=CARTESIAN_POINT('Origin',(-0.01915000000001,-0.00799999999999,-0.0129631448730723));
#33269=CARTESIAN_POINT('Origin',(-0.02115,-0.016,-0.0135625633639073));
#33270=CARTESIAN_POINT('',(-0.02115,-0.024,0.0129631448730623));
#33271=CARTESIAN_POINT('',(-0.02115000000001,-0.02400000000001,-0.0135625633639173));
#33272=CARTESIAN_POINT('',(-0.02115,-0.008,0.0129631448730623));
#33273=CARTESIAN_POINT('',(-0.02115,-0.008,0.0129631448730623));
#33274=CARTESIAN_POINT('',(-0.02115000000001,-0.00799999999999,-0.0135625633639173));
#33275=CARTESIAN_POINT('Origin',(-0.01915,-0.016,0.0129631448730623));
#33276=CARTESIAN_POINT('',(-0.0208062162162162,-0.024,0.0140842817269487));
#33277=CARTESIAN_POINT('Origin',(-0.01915000000001,-0.02400000000001,0.0129631448730723));
#33278=CARTESIAN_POINT('',(-0.0208062162162162,-0.008,0.0140842817269487));
#33279=CARTESIAN_POINT('',(-0.0208062162162381,-0.008,0.0140842817269635));
#33280=CARTESIAN_POINT('Origin',(-0.01915000000001,-0.00799999999999,0.0129631448730723));
#33281=CARTESIAN_POINT('Origin',(-2.55351295663785E-17,-0.016,-3.88578058618804E-17));
#33282=CARTESIAN_POINT('',(-0.0140842817269487,-0.024,0.0208062162162161));
#33283=CARTESIAN_POINT('Origin',(-1.00255351295664E-14,-0.02400000000001,
9.96114219413812E-15));
#33284=CARTESIAN_POINT('',(-0.0140842817269487,-0.008,0.0208062162162161));
#33285=CARTESIAN_POINT('',(-0.0140842817269643,-0.008,0.0208062162162391));
#33286=CARTESIAN_POINT('Origin',(-1.00255351295664E-14,-0.00799999999999,
9.96114219413812E-15));
#33287=CARTESIAN_POINT('Origin',(-0.0129631448730623,-0.016,0.01915));
#33288=CARTESIAN_POINT('',(-0.0129631448730623,-0.024,0.02115));
#33289=CARTESIAN_POINT('Origin',(-0.0129631448730723,-0.02400000000001,
0.01915000000001));
#33290=CARTESIAN_POINT('',(-0.0129631448730623,-0.008,0.02115));
#33291=CARTESIAN_POINT('',(-0.0129631448730623,-0.008,0.0211500000000225));
#33292=CARTESIAN_POINT('Origin',(-0.0129631448730723,-0.00799999999999,
0.01915000000001));
#33293=CARTESIAN_POINT('Origin',(-0.0135625633639073,-0.016,0.02115));
#33294=CARTESIAN_POINT('',(0.0129631448730622,-0.024,0.02115));
#33295=CARTESIAN_POINT('',(-0.0135625633639173,-0.02400000000001,0.0211500000000099));
#33296=CARTESIAN_POINT('',(0.0129631448730622,-0.008,0.02115));
#33297=CARTESIAN_POINT('',(0.0129631448730622,-0.008,0.02115));
#33298=CARTESIAN_POINT('',(-0.0135625633639173,-0.00799999999999,0.0211500000000099));
#33299=CARTESIAN_POINT('Origin',(0.0129631448730622,-0.016,0.01915));
#33300=CARTESIAN_POINT('Origin',(0.0129631448730722,-0.02400000000001,0.01915000000001));
#33301=CARTESIAN_POINT('Origin',(0.0129631448730722,-0.00799999999999,0.01915000000001));
#33302=CARTESIAN_POINT('Origin',(-1.4432899320127E-17,-0.024,-4.10782519111308E-17));
#33303=CARTESIAN_POINT('Origin',(-1.00255351295664E-14,-0.02400000000001,
9.96114219413812E-15));
#33304=CARTESIAN_POINT('',(0.0138,-0.02400000000001,0.0155));
#33305=CARTESIAN_POINT('Origin',(0.01550000000001,-0.02400000000001,0.01550000000001));
#33306=CARTESIAN_POINT('',(-0.0172,-0.02400000000001,-0.0155));
#33307=CARTESIAN_POINT('Origin',(-0.01550000000001,-0.02400000000001,-0.01550000000001));
#33308=CARTESIAN_POINT('',(0.0138,-0.02400000000001,-0.0155));
#33309=CARTESIAN_POINT('Origin',(0.01550000000001,-0.02400000000001,-0.01550000000001));
#33310=CARTESIAN_POINT('',(-0.0172,-0.02400000000001,0.0155));
#33311=CARTESIAN_POINT('Origin',(-0.01550000000001,-0.02400000000001,0.01550000000001));
#33312=CARTESIAN_POINT('',(-0.01915,-0.024,0.00793218971944474));
#33313=CARTESIAN_POINT('',(-0.0079321897194448,-0.024,0.01915));
#33314=CARTESIAN_POINT('',(-0.0079321897194548,-0.02400000000001,0.01915000000001));
#33315=CARTESIAN_POINT('',(0.00793218971944474,-0.024,0.01915));
#33316=CARTESIAN_POINT('',(0.00793218971945474,-0.02400000000001,0.01915000000001));
#33317=CARTESIAN_POINT('',(0.01915,-0.024,0.00793218971944472));
#33318=CARTESIAN_POINT('',(0.01915000000001,-0.02400000000001,0.00793218971945472));
#33319=CARTESIAN_POINT('',(0.01915,-0.024,-0.00793218971944482));
#33320=CARTESIAN_POINT('',(0.01915000000001,-0.02400000000001,-0.00793218971945483));
#33321=CARTESIAN_POINT('',(0.00793218971944474,-0.024,-0.01915));
#33322=CARTESIAN_POINT('',(0.00793218971945474,-0.02400000000001,-0.0191500000000101));
#33323=CARTESIAN_POINT('',(-0.00793218971944481,-0.024,-0.01915));
#33324=CARTESIAN_POINT('',(-0.00793218971945481,-0.02400000000001,-0.0191500000000101));
#33325=CARTESIAN_POINT('',(-0.01915,-0.024,-0.00793218971944481));
#33326=CARTESIAN_POINT('',(-0.01915000000001,-0.02400000000001,-0.00793218971945481));
#33327=CARTESIAN_POINT('',(-0.01915000000001,-0.02400000000001,0.00793218971945474));
#33328=CARTESIAN_POINT('Origin',(-2.55351295663785E-17,-0.016,-3.88578058618804E-17));
#33329=CARTESIAN_POINT('Origin',(-1.00255351295664E-14,-0.00799999999999,
9.96114219413812E-15));
#33330=CARTESIAN_POINT('Origin',(0.0155,-0.0699239856598395,0.0155));
#33331=CARTESIAN_POINT('',(0.0138,-0.00799999999999,0.0155));
#33332=CARTESIAN_POINT('',(0.0138,-0.0699239856598395,0.0155));
#33333=CARTESIAN_POINT('Origin',(0.01550000000001,-0.00799999999999,0.01550000000001));
#33334=CARTESIAN_POINT('Origin',(-0.0155,-0.0699239856598395,-0.0155));
#33335=CARTESIAN_POINT('',(-0.0172,-0.00799999999999,-0.0155));
#33336=CARTESIAN_POINT('',(-0.0172,-0.0699239856598395,-0.0155));
#33337=CARTESIAN_POINT('Origin',(-0.01550000000001,-0.00799999999999,-0.01550000000001));
#33338=CARTESIAN_POINT('Origin',(0.0155,-0.0699239856598395,-0.0155));
#33339=CARTESIAN_POINT('',(0.0138,-0.00799999999999,-0.0155));
#33340=CARTESIAN_POINT('',(0.0138,-0.0699239856598395,-0.0155));
#33341=CARTESIAN_POINT('Origin',(0.01550000000001,-0.00799999999999,-0.01550000000001));
#33342=CARTESIAN_POINT('Origin',(-0.0155,-0.0699239856598395,0.0155));
#33343=CARTESIAN_POINT('',(-0.0172,-0.00799999999999,0.0155));
#33344=CARTESIAN_POINT('',(-0.0172,-0.0699239856598395,0.0155));
#33345=CARTESIAN_POINT('Origin',(-0.01550000000001,-0.00799999999999,0.01550000000001));
#33346=CARTESIAN_POINT('Origin',(0.00793218971944474,-0.016,0.01915));
#33347=CARTESIAN_POINT('',(-0.0079321897194448,-0.008,0.01915));
#33348=CARTESIAN_POINT('',(-0.0079321897194548,-0.016,0.01915000000001));
#33349=CARTESIAN_POINT('',(0.00793218971944474,-0.008,0.01915));
#33350=CARTESIAN_POINT('',(0.00793218971945474,-0.00799999999999,0.01915000000001));
#33351=CARTESIAN_POINT('',(0.00793218971945474,-0.016,0.01915000000001));
#33352=CARTESIAN_POINT('Origin',(0.01915,-0.016,0.00793218971944472));
#33353=CARTESIAN_POINT('',(0.01915,-0.008,0.00793218971944472));
#33354=CARTESIAN_POINT('',(0.01915000000001,-0.00799999999999,0.00793218971945472));
#33355=CARTESIAN_POINT('',(0.01915000000001,-0.016,0.00793218971945472));
#33356=CARTESIAN_POINT('Origin',(0.01915,-0.016,-0.00793218971944482));
#33357=CARTESIAN_POINT('',(0.01915,-0.008,-0.00793218971944482));
#33358=CARTESIAN_POINT('',(0.01915000000001,-0.00799999999999,-0.00793218971945483));
#33359=CARTESIAN_POINT('',(0.01915000000001,-0.016,-0.00793218971945483));
#33360=CARTESIAN_POINT('Origin',(0.00793218971944474,-0.016,-0.01915));
#33361=CARTESIAN_POINT('',(0.00793218971944474,-0.008,-0.01915));
#33362=CARTESIAN_POINT('',(0.00793218971945474,-0.00799999999999,-0.0191500000000101));
#33363=CARTESIAN_POINT('',(0.00793218971945474,-0.016,-0.0191500000000101));
#33364=CARTESIAN_POINT('Origin',(-0.00793218971944481,-0.016,-0.01915));
#33365=CARTESIAN_POINT('',(-0.00793218971944481,-0.008,-0.01915));
#33366=CARTESIAN_POINT('',(-0.00793218971945481,-0.00799999999999,-0.0191500000000101));
#33367=CARTESIAN_POINT('',(-0.00793218971945481,-0.016,-0.0191500000000101));
#33368=CARTESIAN_POINT('Origin',(-0.01915,-0.016,-0.00793218971944481));
#33369=CARTESIAN_POINT('',(-0.01915,-0.008,-0.00793218971944481));
#33370=CARTESIAN_POINT('',(-0.01915000000001,-0.00799999999999,-0.00793218971945481));
#33371=CARTESIAN_POINT('',(-0.01915000000001,-0.016,-0.00793218971945481));
#33372=CARTESIAN_POINT('Origin',(-0.01915,-0.016,0.00793218971944474));
#33373=CARTESIAN_POINT('',(-0.01915,-0.008,0.00793218971944474));
#33374=CARTESIAN_POINT('',(-0.01915000000001,-0.00799999999999,0.00793218971945474));
#33375=CARTESIAN_POINT('',(-0.01915000000001,-0.016,0.00793218971945474));
#33376=CARTESIAN_POINT('Origin',(-0.0079321897194448,-0.016,0.01915));
#33377=CARTESIAN_POINT('',(-0.0079321897194548,-0.00799999999999,0.01915000000001));
#33378=CARTESIAN_POINT('Origin',(-1.4432899320127E-17,-0.008,-4.10782519111308E-17));
#33379=CARTESIAN_POINT('',(0.,0.,0.));
#33380=CARTESIAN_POINT('Origin',(-0.00360121565085295,-0.008,0.0126992616256242));
#33381=CARTESIAN_POINT('',(-0.00384039707060325,-0.008,0.0126265137841014));
#33382=CARTESIAN_POINT('',(-0.00366942049272517,-0.008,0.0129397779442914));
#33383=CARTESIAN_POINT('Origin',(-0.00360121565086296,-0.00799999999999,
0.0126992616256342));
#33384=CARTESIAN_POINT('',(-0.00366942049272517,-0.024,0.0129397779442914));
#33385=CARTESIAN_POINT('',(-0.00366942049273517,-0.00799999999999,0.0129397779443014));
#33386=CARTESIAN_POINT('',(-0.00384039707060325,-0.024,0.0126265137841014));
#33387=CARTESIAN_POINT('Origin',(-0.00360121565086296,-0.02400000000001,
0.0126992616256342));
#33388=CARTESIAN_POINT('',(-0.00384039707061325,-0.00799999999999,0.0126265137841114));
#33389=CARTESIAN_POINT('Origin',(-4.44089209850063E-17,-0.008,6.72997231505748E-33));
#33390=CARTESIAN_POINT('',(-0.00329207760827854,-0.008,0.0130408866654485));
#33391=CARTESIAN_POINT('Origin',(-4.44089209850063E-17,-0.00799999999999,
6.72997231505748E-33));
#33392=CARTESIAN_POINT('',(-0.00329207760827854,-0.024,0.0130408866654485));
#33393=CARTESIAN_POINT('',(-0.00329207760828854,-0.00799999999999,0.0130408866654585));
#33394=CARTESIAN_POINT('Origin',(-4.44089209850063E-17,-0.02400000000001,
6.72997231505748E-33));
#33395=CARTESIAN_POINT('Origin',(-0.00323088657466742,-0.008,0.0127984910025219));
#33396=CARTESIAN_POINT('',(-0.00298737546828901,-0.008,0.0128550802335678));
#33397=CARTESIAN_POINT('Origin',(-0.00323088657467743,-0.00799999999999,
0.0127984910025319));
#33398=CARTESIAN_POINT('',(-0.00298737546828901,-0.024,0.0128550802335678));
#33399=CARTESIAN_POINT('',(-0.00298737546829902,-0.00799999999999,0.0128550802335778));
#33400=CARTESIAN_POINT('Origin',(-0.00323088657467743,-0.02400000000001,
0.0127984910025319));
#33401=CARTESIAN_POINT('Origin',(-0.00294264001438606,-0.008,0.0126625775316771));
#33402=CARTESIAN_POINT('',(-0.00294264001438606,-0.008,0.0126625775316771));
#33403=CARTESIAN_POINT('',(-0.00291295831081416,-0.00799999999999,0.0125348531511851));
#33404=CARTESIAN_POINT('',(-0.00294264001438606,-0.024,0.0126625775316771));
#33405=CARTESIAN_POINT('',(-0.00294264001439606,-0.016,0.0126625775316871));
#33406=CARTESIAN_POINT('',(-0.00291295831081416,-0.02400000000001,0.0125348531511851));
#33407=CARTESIAN_POINT('Origin',(-0.00191282048773815,-0.008,0.0130606706482359));
#33408=CARTESIAN_POINT('',(-0.00215945117603188,-0.008,0.0130197646145518));
#33409=CARTESIAN_POINT('',(-0.00194904814849077,-0.008,0.0133080318347555));
#33410=CARTESIAN_POINT('Origin',(-0.00191282048774815,-0.00799999999999,
0.0130606706482459));
#33411=CARTESIAN_POINT('',(-0.00194904814849077,-0.024,0.0133080318347555));
#33412=CARTESIAN_POINT('',(-0.00194904814850077,-0.00799999999999,0.0133080318347655));
#33413=CARTESIAN_POINT('',(-0.00215945117603188,-0.024,0.0130197646145518));
#33414=CARTESIAN_POINT('Origin',(-0.00191282048774815,-0.02400000000001,
0.0130606706482459));
#33415=CARTESIAN_POINT('',(-0.00215945117604188,-0.00799999999999,0.0130197646145618));
#33416=CARTESIAN_POINT('Origin',(-4.44089209850063E-17,-0.008,6.72997231505748E-33));
#33417=CARTESIAN_POINT('',(-0.00156173614835732,-0.008,0.0133590224269186));
#33418=CARTESIAN_POINT('Origin',(-4.44089209850063E-17,-0.00799999999999,
6.72997231505748E-33));
#33419=CARTESIAN_POINT('',(-0.00156173614835732,-0.024,0.0133590224269186));
#33420=CARTESIAN_POINT('',(-0.00156173614836731,-0.00799999999999,0.0133590224269286));
#33421=CARTESIAN_POINT('Origin',(-4.44089209850063E-17,-0.02400000000001,
6.72997231505748E-33));
#33422=CARTESIAN_POINT('Origin',(-0.00153270759541388,-0.008,0.0131107134598755));
#33423=CARTESIAN_POINT('',(-0.00128389338345847,-0.008,0.0131350339847262));
#33424=CARTESIAN_POINT('Origin',(-0.00153270759542387,-0.00799999999999,
0.0131107134598855));
#33425=CARTESIAN_POINT('',(-0.00128389338345847,-0.024,0.0131350339847262));
#33426=CARTESIAN_POINT('',(-0.00128389338346847,-0.00799999999999,0.0131350339847362));
#33427=CARTESIAN_POINT('Origin',(-0.00153270759542387,-0.02400000000001,
0.0131107134598855));
#33428=CARTESIAN_POINT('Origin',(-0.00126466729223502,-0.008,0.0129383390216809));
#33429=CARTESIAN_POINT('',(-0.00126466729223502,-0.008,0.0129383390216809));
#33430=CARTESIAN_POINT('',(-0.00126540384839645,-0.00799999999999,0.0129458744527519));
#33431=CARTESIAN_POINT('',(-0.00126466729223502,-0.024,0.0129383390216809));
#33432=CARTESIAN_POINT('',(-0.00126466729224502,-0.016,0.0129383390216909));
#33433=CARTESIAN_POINT('',(-0.00126540384839645,-0.02400000000001,0.0129458744527519));
#33434=CARTESIAN_POINT('Origin',(-0.000191696435744125,-0.008,0.0131986079749541));
#33435=CARTESIAN_POINT('',(-0.000441556473125634,-0.008,0.0131902436626865));
#33436=CARTESIAN_POINT('',(-0.00019532705005746,-0.008,0.0134485816108434));
#33437=CARTESIAN_POINT('Origin',(-0.000191696435754125,-0.00799999999999,
0.0131986079749641));
#33438=CARTESIAN_POINT('',(-0.00019532705005746,-0.024,0.0134485816108434));
#33439=CARTESIAN_POINT('',(-0.00019532705006746,-0.00799999999999,0.0134485816108534));
#33440=CARTESIAN_POINT('',(-0.000441556473125634,-0.024,0.0131902436626865));
#33441=CARTESIAN_POINT('Origin',(-0.000191696435754125,-0.02400000000001,
0.0131986079749641));
#33442=CARTESIAN_POINT('',(-0.000441556473135633,-0.00799999999999,0.0131902436626965));
#33443=CARTESIAN_POINT('Origin',(-4.44089209850063E-17,-0.008,6.72997231505748E-33));
#33444=CARTESIAN_POINT('',(0.000195327050057369,-0.008,0.0134485816108434));
#33445=CARTESIAN_POINT('Origin',(-4.44089209850063E-17,-0.00799999999999,
6.72997231505748E-33));
#33446=CARTESIAN_POINT('',(0.000195327050057369,-0.024,0.0134485816108434));
#33447=CARTESIAN_POINT('',(0.000195327050067369,-0.00799999999999,0.0134485816108534));
#33448=CARTESIAN_POINT('Origin',(-4.44089209850063E-17,-0.02400000000001,
6.72997231505748E-33));
#33449=CARTESIAN_POINT('Origin',(0.000191696435744034,-0.008,0.0131986079749541));
#33450=CARTESIAN_POINT('',(0.000441556473125544,-0.008,0.0131902436626865));
#33451=CARTESIAN_POINT('Origin',(0.000191696435754034,-0.00799999999999,
0.0131986079749641));
#33452=CARTESIAN_POINT('',(0.000441556473125544,-0.024,0.0131902436626865));
#33453=CARTESIAN_POINT('',(0.000441556473135544,-0.00799999999999,0.0131902436626965));
#33454=CARTESIAN_POINT('Origin',(0.000191696435754034,-0.02400000000001,
0.0131986079749641));
#33455=CARTESIAN_POINT('Origin',(0.000434944237918172,-0.008,0.0129927219438385));
#33456=CARTESIAN_POINT('',(0.000434944237918172,-0.008,0.0129927219438385));
#33457=CARTESIAN_POINT('',(0.000436112706128989,-0.00799999999999,0.0130276266077339));
#33458=CARTESIAN_POINT('',(0.000434944237918172,-0.024,0.0129927219438385));
#33459=CARTESIAN_POINT('',(0.000434944237928171,-0.016,0.0129927219438485));
#33460=CARTESIAN_POINT('',(0.000436112706128989,-0.02400000000001,0.0130276266077339));
#33461=CARTESIAN_POINT('Origin',(0.00153270759541378,-0.008,0.0131107134598755));
#33462=CARTESIAN_POINT('',(0.00128389338345839,-0.008,0.0131350339847262));
#33463=CARTESIAN_POINT('',(0.00156173614835723,-0.008,0.0133590224269186));
#33464=CARTESIAN_POINT('Origin',(0.00153270759542378,-0.00799999999999,
0.0131107134598855));
#33465=CARTESIAN_POINT('',(0.00156173614835723,-0.024,0.0133590224269186));
#33466=CARTESIAN_POINT('',(0.00156173614836722,-0.00799999999999,0.0133590224269286));
#33467=CARTESIAN_POINT('',(0.00128389338345839,-0.024,0.0131350339847262));
#33468=CARTESIAN_POINT('Origin',(0.00153270759542378,-0.02400000000001,
0.0131107134598855));
#33469=CARTESIAN_POINT('',(0.00128389338346839,-0.00799999999999,0.0131350339847362));
#33470=CARTESIAN_POINT('Origin',(-4.44089209850063E-17,-0.008,6.72997231505748E-33));
#33471=CARTESIAN_POINT('',(0.00194904814849068,-0.008,0.0133080318347555));
#33472=CARTESIAN_POINT('Origin',(-4.44089209850063E-17,-0.00799999999999,
6.72997231505748E-33));
#33473=CARTESIAN_POINT('',(0.00194904814849068,-0.024,0.0133080318347555));
#33474=CARTESIAN_POINT('',(0.00194904814850068,-0.00799999999999,0.0133080318347655));
#33475=CARTESIAN_POINT('Origin',(-4.44089209850063E-17,-0.02400000000001,
6.72997231505748E-33));
#33476=CARTESIAN_POINT('Origin',(0.00191282048773806,-0.008,0.0130606706482359));
#33477=CARTESIAN_POINT('',(0.00215945117603179,-0.008,0.0130197646145518));
#33478=CARTESIAN_POINT('Origin',(0.00191282048774806,-0.00799999999999,
0.0130606706482459));
#33479=CARTESIAN_POINT('',(0.00215945117603179,-0.024,0.0130197646145518));
#33480=CARTESIAN_POINT('',(0.0021594511760418,-0.00799999999999,0.0130197646145618));
#33481=CARTESIAN_POINT('Origin',(0.00191282048774806,-0.02400000000001,
0.0130606706482459));
#33482=CARTESIAN_POINT('Origin',(0.00212711375157126,-0.008,0.0128247957912739));
#33483=CARTESIAN_POINT('',(0.00212711375157126,-0.008,0.0128247957912739));
#33484=CARTESIAN_POINT('',(0.00211900825769009,-0.00799999999999,0.0127759261415696));
#33485=CARTESIAN_POINT('',(0.00212711375157126,-0.024,0.0128247957912739));
#33486=CARTESIAN_POINT('',(0.00212711375158127,-0.016,0.0128247957912839));
#33487=CARTESIAN_POINT('',(0.00211900825769009,-0.02400000000001,0.0127759261415696));
#33488=CARTESIAN_POINT('Origin',(0.00323088657466734,-0.008,0.0127984910025219));
#33489=CARTESIAN_POINT('',(0.00298737546828893,-0.008,0.0128550802335678));
#33490=CARTESIAN_POINT('',(0.00329207760827845,-0.008,0.0130408866654485));
#33491=CARTESIAN_POINT('Origin',(0.00323088657467733,-0.00799999999999,
0.0127984910025319));
#33492=CARTESIAN_POINT('',(0.00329207760827845,-0.024,0.0130408866654485));
#33493=CARTESIAN_POINT('',(0.00329207760828845,-0.00799999999999,0.0130408866654585));
#33494=CARTESIAN_POINT('',(0.00298737546828893,-0.024,0.0128550802335678));
#33495=CARTESIAN_POINT('Origin',(0.00323088657467733,-0.02400000000001,
0.0127984910025319));
#33496=CARTESIAN_POINT('',(0.00298737546829892,-0.00799999999999,0.0128550802335778));
#33497=CARTESIAN_POINT('Origin',(-4.44089209850063E-17,-0.008,6.72997231505748E-33));
#33498=CARTESIAN_POINT('',(0.00366942049272508,-0.008,0.0129397779442914));
#33499=CARTESIAN_POINT('Origin',(-4.44089209850063E-17,-0.00799999999999,
6.72997231505748E-33));
#33500=CARTESIAN_POINT('',(0.00366942049272508,-0.024,0.0129397779442914));
#33501=CARTESIAN_POINT('',(0.00366942049273508,-0.00799999999999,0.0129397779443014));
#33502=CARTESIAN_POINT('Origin',(-4.44089209850063E-17,-0.02400000000001,
6.72997231505748E-33));
#33503=CARTESIAN_POINT('Origin',(0.00360121565085287,-0.008,0.0126992616256242));
#33504=CARTESIAN_POINT('',(0.00384039707060316,-0.008,0.0126265137841014));
#33505=CARTESIAN_POINT('Origin',(0.00360121565086286,-0.00799999999999,
0.0126992616256342));
#33506=CARTESIAN_POINT('',(0.00384039707060316,-0.024,0.0126265137841014));
#33507=CARTESIAN_POINT('',(0.00384039707061316,-0.00799999999999,0.0126265137841114));
#33508=CARTESIAN_POINT('Origin',(0.00360121565086286,-0.02400000000001,
0.0126992616256342));
#33509=CARTESIAN_POINT('Origin',(0.00378288775918762,-0.008,0.0124374338270155));
#33510=CARTESIAN_POINT('',(0.00378288775918762,-0.008,0.0124374338270155));
#33511=CARTESIAN_POINT('',(0.00371177878877259,-0.00799999999999,0.0122036407116943));
#33512=CARTESIAN_POINT('',(0.00378288775918762,-0.024,0.0124374338270155));
#33513=CARTESIAN_POINT('',(0.00378288775919761,-0.016,0.0124374338270255));
#33514=CARTESIAN_POINT('',(0.00371177878877259,-0.02400000000001,0.0122036407116943));
#33515=CARTESIAN_POINT('Origin',(0.00304450063026857,-0.008,0.0131008975231583));
#33516=CARTESIAN_POINT('',(0.00294264001438597,-0.024,0.0126625775316771));
#33517=CARTESIAN_POINT('',(0.00296388861875537,-0.02400000000001,0.0127540131469256));
#33518=CARTESIAN_POINT('',(0.00294264001438597,-0.008,0.0126625775316771));
#33519=CARTESIAN_POINT('',(0.00294264001439597,-0.016,0.0126625775316871));
#33520=CARTESIAN_POINT('',(0.00296388861875537,-0.00799999999999,0.0127540131469256));
#33521=CARTESIAN_POINT('Origin',(0.00130844423696615,-0.008,0.0133862046032006));
#33522=CARTESIAN_POINT('',(0.00126466729223494,-0.024,0.0129383390216809));
#33523=CARTESIAN_POINT('',(0.00128729232076197,-0.02400000000001,0.0131698072435117));
#33524=CARTESIAN_POINT('',(0.00126466729223494,-0.008,0.0129383390216809));
#33525=CARTESIAN_POINT('',(0.00126466729224494,-0.016,0.0129383390216909));
#33526=CARTESIAN_POINT('',(0.00128729232076197,-0.00799999999999,0.0131698072435117));
#33527=CARTESIAN_POINT('Origin',(-0.00220074461220267,-0.008,0.0132687310302026));
#33528=CARTESIAN_POINT('',(-0.00212711375157135,-0.024,0.0128247957912739));
#33529=CARTESIAN_POINT('',(-0.00215582368800584,-0.02400000000001,0.0129978937610339));
#33530=CARTESIAN_POINT('',(-0.00212711375157135,-0.008,0.0128247957912739));
#33531=CARTESIAN_POINT('',(-0.00212711375158134,-0.016,0.0128247957912839));
#33532=CARTESIAN_POINT('',(-0.00215582368800584,-0.00799999999999,0.0129978937610339));
#33533=CARTESIAN_POINT('Origin',(-0.00391383387392881,-0.008,0.012867960382566));
#33534=CARTESIAN_POINT('',(-0.0037828877591877,-0.024,0.0124374338270155));
#33535=CARTESIAN_POINT('',(-0.00377725184614322,-0.02400000000001,0.0124189039894696));
#33536=CARTESIAN_POINT('',(-0.0037828877591877,-0.008,0.0124374338270155));
#33537=CARTESIAN_POINT('',(-0.00378288775919771,-0.016,0.0124374338270255));
#33538=CARTESIAN_POINT('',(-0.00377725184614322,-0.00799999999999,0.0124189039894696));
#33539=CARTESIAN_POINT('Origin',(-4.44089209850063E-17,-0.016,6.72997231505748E-33));
#33540=CARTESIAN_POINT('',(0.00433948917003898,-0.008,0.0122543393841983));
#33541=CARTESIAN_POINT('Origin',(-4.44089209850063E-17,-0.00799999999999,
6.72997231505748E-33));
#33542=CARTESIAN_POINT('',(0.00433948917003898,-0.024,0.0122543393841983));
#33543=CARTESIAN_POINT('',(0.00433948917004898,-0.016,0.0122543393842083));
#33544=CARTESIAN_POINT('Origin',(-4.44089209850063E-17,-0.02400000000001,
6.72997231505748E-33));
#33545=CARTESIAN_POINT('Origin',(-4.44089209850063E-17,-0.016,6.72997231505748E-33));
#33546=CARTESIAN_POINT('Origin',(-4.44089209850063E-17,-0.02400000000001,
6.72997231505748E-33));
#33547=CARTESIAN_POINT('Origin',(-4.44089209850063E-17,-0.00799999999999,
6.72997231505748E-33));
#33548=CARTESIAN_POINT('Origin',(-4.57966997657877E-17,-0.024,0.0130771696920992));
#33549=CARTESIAN_POINT('',(0.00463991534334938,-0.024,0.0131027167261813));
#33550=CARTESIAN_POINT('',(0.00463991534335938,-0.02400000000001,0.0131027167261913));
#33551=CARTESIAN_POINT('',(-0.00463991534334946,-0.024,0.0131027167261813));
#33552=CARTESIAN_POINT('Origin',(-4.44089209850063E-17,-0.02400000000001,
6.72997231505748E-33));
#33553=CARTESIAN_POINT('',(-0.00433948917003908,-0.024,0.0122543393841983));
#33554=CARTESIAN_POINT('',(-0.00433948917004908,-0.02400000000001,0.0122543393842083));
#33555=CARTESIAN_POINT('Origin',(-4.44089209850063E-17,-0.02400000000001,
6.72997231505748E-33));
#33556=CARTESIAN_POINT('Origin',(-4.44089209850063E-17,-0.02400000000001,
6.72997231505748E-33));
#33557=CARTESIAN_POINT('',(-0.00043494423791826,-0.024,0.0129927219438385));
#33558=CARTESIAN_POINT('Origin',(-4.44089209850063E-17,-0.02400000000001,
6.72997231505748E-33));
#33559=CARTESIAN_POINT('',(-0.000443640587169973,-0.02400000000001,0.0132525006413773));
#33560=CARTESIAN_POINT('Origin',(-4.44089209850063E-17,-0.02400000000001,
6.72997231505748E-33));
#33561=CARTESIAN_POINT('Origin',(-4.44089209850063E-17,-0.016,6.72997231505748E-33));
#33562=CARTESIAN_POINT('',(-0.00043494423791826,-0.008,0.0129927219438385));
#33563=CARTESIAN_POINT('Origin',(-4.44089209850063E-17,-0.00799999999999,
6.72997231505748E-33));
#33564=CARTESIAN_POINT('',(-0.000434944237928261,-0.016,0.0129927219438485));
#33565=CARTESIAN_POINT('Origin',(-4.44089209850063E-17,-0.016,6.72997231505748E-33));
#33566=CARTESIAN_POINT('',(-0.00433948917003908,-0.008,0.0122543393841983));
#33567=CARTESIAN_POINT('',(-0.00433948917004908,-0.016,0.0122543393842083));
#33568=CARTESIAN_POINT('Origin',(-4.44089209850063E-17,-0.00799999999999,
6.72997231505748E-33));
#33569=CARTESIAN_POINT('Origin',(-0.000450000000000044,-0.008,0.0134424700111252));
#33570=CARTESIAN_POINT('',(-0.000443640587169973,-0.00799999999999,0.0132525006413773));
#33571=CARTESIAN_POINT('Origin',(-4.44089209850063E-17,-0.016,6.72997231505748E-33));
#33572=CARTESIAN_POINT('Origin',(-4.44089209850063E-17,-0.00799999999999,
6.72997231505748E-33));
#33573=CARTESIAN_POINT('Origin',(-4.44089209850063E-17,-0.016,6.72997231505748E-33));
#33574=CARTESIAN_POINT('',(0.00463991534334938,-0.008,0.0131027167261813));
#33575=CARTESIAN_POINT('',(0.00463991534335938,-0.016,0.0131027167261913));
#33576=CARTESIAN_POINT('',(-0.00463991534334946,-0.008,0.0131027167261813));
#33577=CARTESIAN_POINT('Origin',(-4.44089209850063E-17,-0.00799999999999,
6.72997231505748E-33));
#33578=CARTESIAN_POINT('',(-0.00463991534335947,-0.016,0.0131027167261913));
#33579=CARTESIAN_POINT('Origin',(-0.00433948917003908,-0.016,0.0122543393841983));
#33580=CARTESIAN_POINT('',(-0.00433948917004908,-0.00799999999999,0.0122543393842083));
#33581=CARTESIAN_POINT('Origin',(-4.44089209850063E-17,-0.016,6.72997231505748E-33));
#33582=CARTESIAN_POINT('Origin',(-4.44089209850063E-17,-0.00799999999999,
6.72997231505748E-33));
#33583=CARTESIAN_POINT('Origin',(0.00463991534334938,-0.016,0.0131027167261813));
#33584=CARTESIAN_POINT('',(0.00463991534335938,-0.00799999999999,0.0131027167261913));
#33585=CARTESIAN_POINT('Origin',(-4.57966997657877E-17,-0.008,0.0130771696920992));
#33586=CARTESIAN_POINT('',(0.,0.,0.));
#33587=CARTESIAN_POINT('Origin',(0.0262,-0.02495,0.00124999999999987));
#33588=CARTESIAN_POINT('',(0.02115,-0.02495,0.000749999999999928));
#33589=CARTESIAN_POINT('',(0.02115,-0.02495,0.00124999999999993));
#33590=CARTESIAN_POINT('',(0.02115000000001,-0.02495000000001,-0.00524999999999003));
#33591=CARTESIAN_POINT('',(0.0229,-0.02495,0.000749999999999909));
#33592=CARTESIAN_POINT('',(0.0262000000000101,-0.02495000000001,0.000750000000009974));
#33593=CARTESIAN_POINT('',(0.0229,-0.02495,0.00124999999999991));
#33594=CARTESIAN_POINT('',(0.0229000000000101,-0.02495000000001,0.00377500000000991));
#33595=CARTESIAN_POINT('',(0.0262000000000101,-0.02495000000001,0.00125000000000997));
#33596=CARTESIAN_POINT('Origin',(0.0262,-0.02545,0.00124999999999987));
#33597=CARTESIAN_POINT('',(0.02115,-0.02545,0.00124999999999993));
#33598=CARTESIAN_POINT('',(0.0211500000000101,-0.02387500000001,0.00125000000000993));
#33599=CARTESIAN_POINT('',(0.0229,-0.02545,0.00124999999999991));
#33600=CARTESIAN_POINT('',(0.0229000000000101,-0.0247750000000099,0.00125000000000991));
#33601=CARTESIAN_POINT('',(0.0262000000000101,-0.02545000000001,0.00125000000000997));
#33602=CARTESIAN_POINT('Origin',(0.0262,-0.02545,0.000749999999999874));
#33603=CARTESIAN_POINT('',(0.02115,-0.02545,0.000749999999999928));
#33604=CARTESIAN_POINT('',(0.02115000000001,-0.02545000000001,-0.00549999999999003));
#33605=CARTESIAN_POINT('',(0.0229,-0.02545,0.000749999999999909));
#33606=CARTESIAN_POINT('',(0.0229000000000101,-0.02545000000001,0.00352500000000991));
#33607=CARTESIAN_POINT('',(0.0262000000000101,-0.02545000000001,0.000750000000009974));
#33608=CARTESIAN_POINT('Origin',(0.0262,-0.02495,0.000749999999999874));
#33609=CARTESIAN_POINT('',(0.0211500000000101,-0.02362500000001,0.000750000000009929));
#33610=CARTESIAN_POINT('',(0.0229000000000101,-0.02452500000001,0.000750000000009909));
#33611=CARTESIAN_POINT('Origin',(0.0262,-0.02545,-0.00475000000000013));
#33612=CARTESIAN_POINT('',(0.02115,-0.02495,-0.00475000000000007));
#33613=CARTESIAN_POINT('',(0.02115,-0.02545,-0.00475000000000007));
#33614=CARTESIAN_POINT('',(0.02115000000001,-0.02387500000001,-0.00474999999999007));
#33615=CARTESIAN_POINT('',(0.0229,-0.02495,-0.00475000000000009));
#33616=CARTESIAN_POINT('',(0.0262000000000101,-0.02495000000001,-0.00474999999999007));
#33617=CARTESIAN_POINT('',(0.0229,-0.02545,-0.00475000000000009));
#33618=CARTESIAN_POINT('',(0.0229000000000101,-0.02477500000001,-0.00474999999999007));
#33619=CARTESIAN_POINT('',(0.0262000000000101,-0.02545000000001,-0.00474999999999007));
#33620=CARTESIAN_POINT('Origin',(0.0262,-0.02545,-0.00525000000000013));
#33621=CARTESIAN_POINT('',(0.02115,-0.02545,-0.00525000000000007));
#33622=CARTESIAN_POINT('',(0.0211500000000101,-0.02545000000001,-0.00849999999999003));
#33623=CARTESIAN_POINT('',(0.0229,-0.02545,-0.00525000000000009));
#33624=CARTESIAN_POINT('',(0.0229000000000101,-0.02545000000001,0.000525000000009908));
#33625=CARTESIAN_POINT('',(0.0262000000000101,-0.02545000000001,-0.00524999999999008));
#33626=CARTESIAN_POINT('Origin',(0.0262,-0.02495,-0.00525000000000013));
#33627=CARTESIAN_POINT('',(0.02115,-0.02495,-0.00525000000000007));
#33628=CARTESIAN_POINT('',(0.0211500000000101,-0.02362500000001,-0.00524999999999007));
#33629=CARTESIAN_POINT('',(0.0229,-0.02495,-0.00525000000000009));
#33630=CARTESIAN_POINT('',(0.0229000000000101,-0.02452500000001,-0.00524999999999007));
#33631=CARTESIAN_POINT('',(0.0262000000000101,-0.02495000000001,-0.00524999999999008));
#33632=CARTESIAN_POINT('Origin',(0.0262,-0.02495,-0.00475000000000013));
#33633=CARTESIAN_POINT('',(0.0211500000000101,-0.02495000000001,-0.00824999999999003));
#33634=CARTESIAN_POINT('',(0.0229000000000101,-0.02495000000001,0.000775000000009908));
#33635=CARTESIAN_POINT('Origin',(0.0262,-0.02495,0.00274999999999987));
#33636=CARTESIAN_POINT('',(0.02115,-0.02545,0.00274999999999993));
#33637=CARTESIAN_POINT('',(0.02115,-0.02495,0.00274999999999993));
#33638=CARTESIAN_POINT('',(0.02115000000001,-0.02362500000001,0.00275000000000993));
#33639=CARTESIAN_POINT('',(0.0229,-0.02545,0.00274999999999991));
#33640=CARTESIAN_POINT('',(0.0262000000000101,-0.02545000000001,0.00275000000000997));
#33641=CARTESIAN_POINT('',(0.0229,-0.02495,0.00274999999999991));
#33642=CARTESIAN_POINT('',(0.0229000000000101,-0.02452500000001,0.00275000000000991));
#33643=CARTESIAN_POINT('',(0.0262000000000101,-0.02495000000001,0.00275000000000997));
#33644=CARTESIAN_POINT('Origin',(0.0262,-0.02495,0.00324999999999987));
#33645=CARTESIAN_POINT('',(0.02115,-0.02495,0.00324999999999992));
#33646=CARTESIAN_POINT('',(0.02115000000001,-0.02495000000001,-0.00424999999999004));
#33647=CARTESIAN_POINT('',(0.0229,-0.02495,0.00324999999999991));
#33648=CARTESIAN_POINT('',(0.0229000000000101,-0.02495000000001,0.00477500000000991));
#33649=CARTESIAN_POINT('',(0.0262000000000101,-0.02495000000001,0.00325000000000997));
#33650=CARTESIAN_POINT('Origin',(0.0262,-0.02545,0.00324999999999987));
#33651=CARTESIAN_POINT('',(0.02115,-0.02545,0.00324999999999992));
#33652=CARTESIAN_POINT('',(0.0211500000000101,-0.02387500000001,0.00325000000000992));
#33653=CARTESIAN_POINT('',(0.0229,-0.02545,0.00324999999999991));
#33654=CARTESIAN_POINT('',(0.0229000000000101,-0.02477500000001,0.00325000000000991));
#33655=CARTESIAN_POINT('',(0.0262000000000101,-0.02545000000001,0.00325000000000997));
#33656=CARTESIAN_POINT('Origin',(0.0262,-0.02545,0.00274999999999987));
#33657=CARTESIAN_POINT('',(0.0211500000000101,-0.02545000000001,-0.00449999999999003));
#33658=CARTESIAN_POINT('',(0.0229000000000101,-0.02545000000001,0.00452500000000991));
#33659=CARTESIAN_POINT('Origin',(0.0262,-0.02495,-0.000750000000000127));
#33660=CARTESIAN_POINT('',(0.02115,-0.02495,-0.00125000000000007));
#33661=CARTESIAN_POINT('',(0.02115,-0.02495,-0.000750000000000074));
#33662=CARTESIAN_POINT('',(0.02115000000001,-0.02495000000001,-0.00624999999999003));
#33663=CARTESIAN_POINT('',(0.0229,-0.02495,-0.00125000000000009));
#33664=CARTESIAN_POINT('',(0.0262000000000102,-0.02495000000001,-0.00124999999999003));
#33665=CARTESIAN_POINT('',(0.0229,-0.02495,-0.000750000000000093));
#33666=CARTESIAN_POINT('',(0.0229000000000101,-0.02495000000001,0.00277500000000991));
#33667=CARTESIAN_POINT('',(0.0262000000000101,-0.02495000000001,-0.000749999999990028));
#33668=CARTESIAN_POINT('Origin',(0.0262,-0.02545,-0.000750000000000127));
#33669=CARTESIAN_POINT('',(0.02115,-0.02545,-0.000750000000000074));
#33670=CARTESIAN_POINT('',(0.0211500000000101,-0.02387500000001,-0.000749999999990073));
#33671=CARTESIAN_POINT('',(0.0229,-0.02545,-0.000750000000000093));
#33672=CARTESIAN_POINT('',(0.0229000000000101,-0.02477500000001,-0.000749999999990092));
#33673=CARTESIAN_POINT('',(0.0262000000000101,-0.02545000000001,-0.000749999999990028));
#33674=CARTESIAN_POINT('Origin',(0.0262,-0.02545,-0.00125000000000013));
#33675=CARTESIAN_POINT('',(0.02115,-0.02545,-0.00125000000000007));
#33676=CARTESIAN_POINT('',(0.02115000000001,-0.02545000000001,-0.00649999999999003));
#33677=CARTESIAN_POINT('',(0.0229,-0.02545,-0.00125000000000009));
#33678=CARTESIAN_POINT('',(0.0229000000000101,-0.02545000000001,0.00252500000000991));
#33679=CARTESIAN_POINT('',(0.0262000000000102,-0.02545000000001,-0.00124999999999003));
#33680=CARTESIAN_POINT('Origin',(0.0262,-0.02495,-0.00125000000000013));
#33681=CARTESIAN_POINT('',(0.0211500000000101,-0.02362500000001,-0.00124999999999007));
#33682=CARTESIAN_POINT('',(0.0229000000000101,-0.02452500000001,-0.00124999999999009));
#33683=CARTESIAN_POINT('Origin',(0.0262,-0.02545,-0.00325000000000012));
#33684=CARTESIAN_POINT('',(0.02115,-0.02545,-0.00275000000000007));
#33685=CARTESIAN_POINT('',(0.02115,-0.02545,-0.00325000000000007));
#33686=CARTESIAN_POINT('',(0.0211500000000101,-0.02545000000001,-0.00749999999999003));
#33687=CARTESIAN_POINT('',(0.0229,-0.02545,-0.00275000000000009));
#33688=CARTESIAN_POINT('',(0.0262000000000101,-0.02545000000001,-0.00274999999999008));
#33689=CARTESIAN_POINT('',(0.0229,-0.02545,-0.00325000000000009));
#33690=CARTESIAN_POINT('',(0.0229000000000101,-0.02545000000001,0.00152500000000991));
#33691=CARTESIAN_POINT('',(0.0262000000000101,-0.02545000000001,-0.00324999999999008));
#33692=CARTESIAN_POINT('Origin',(0.0262,-0.02495,-0.00325000000000012));
#33693=CARTESIAN_POINT('',(0.02115,-0.02495,-0.00325000000000007));
#33694=CARTESIAN_POINT('',(0.0211500000000101,-0.02362500000001,-0.00324999999999007));
#33695=CARTESIAN_POINT('',(0.0229,-0.02495,-0.00325000000000009));
#33696=CARTESIAN_POINT('',(0.0229000000000101,-0.02452500000001,-0.00324999999999007));
#33697=CARTESIAN_POINT('',(0.0262000000000101,-0.02495000000001,-0.00324999999999008));
#33698=CARTESIAN_POINT('Origin',(0.0262,-0.02495,-0.00275000000000013));
#33699=CARTESIAN_POINT('',(0.02115,-0.02495,-0.00275000000000007));
#33700=CARTESIAN_POINT('',(0.0211500000000101,-0.02495000000001,-0.00724999999999003));
#33701=CARTESIAN_POINT('',(0.0229,-0.02495,-0.00275000000000009));
#33702=CARTESIAN_POINT('',(0.0229000000000101,-0.02495000000001,0.00177500000000991));
#33703=CARTESIAN_POINT('',(0.0262000000000101,-0.02495000000001,-0.00274999999999007));
#33704=CARTESIAN_POINT('Origin',(0.0262,-0.02545,-0.00275000000000013));
#33705=CARTESIAN_POINT('',(0.02115000000001,-0.02387500000001,-0.00274999999999007));
#33706=CARTESIAN_POINT('',(0.0229000000000101,-0.0247750000000099,-0.00274999999999008));
#33707=CARTESIAN_POINT('Origin',(0.0262,-0.02545,0.00474999999999988));
#33708=CARTESIAN_POINT('',(0.02115,-0.02545,0.00524999999999993));
#33709=CARTESIAN_POINT('',(0.02115,-0.02545,0.00474999999999993));
#33710=CARTESIAN_POINT('',(0.02115000000001,-0.02545000000001,-0.00349999999999003));
#33711=CARTESIAN_POINT('',(0.0229,-0.02545,0.00524999999999991));
#33712=CARTESIAN_POINT('',(0.0262000000000101,-0.02545000000001,0.00525000000000998));
#33713=CARTESIAN_POINT('',(0.0229,-0.02545,0.00474999999999991));
#33714=CARTESIAN_POINT('',(0.0229000000000101,-0.02545000000001,0.00552500000000991));
#33715=CARTESIAN_POINT('',(0.0262000000000101,-0.02545000000001,0.00475000000000998));
#33716=CARTESIAN_POINT('Origin',(0.0262,-0.02495,0.00474999999999988));
#33717=CARTESIAN_POINT('',(0.02115,-0.02495,0.00474999999999993));
#33718=CARTESIAN_POINT('',(0.02115000000001,-0.02362500000001,0.00475000000000993));
#33719=CARTESIAN_POINT('',(0.0229,-0.02495,0.00474999999999991));
#33720=CARTESIAN_POINT('',(0.0229000000000101,-0.02452500000001,0.00475000000000991));
#33721=CARTESIAN_POINT('',(0.0262000000000101,-0.02495000000001,0.00475000000000998));
#33722=CARTESIAN_POINT('Origin',(0.0262,-0.02495,0.00524999999999988));
#33723=CARTESIAN_POINT('',(0.02115,-0.02495,0.00524999999999993));
#33724=CARTESIAN_POINT('',(0.02115000000001,-0.02495000000001,-0.00324999999999003));
#33725=CARTESIAN_POINT('',(0.0229,-0.02495,0.00524999999999991));
#33726=CARTESIAN_POINT('',(0.0229000000000101,-0.02495000000001,0.00577500000000991));
#33727=CARTESIAN_POINT('',(0.0262000000000101,-0.02495000000001,0.00525000000000998));
#33728=CARTESIAN_POINT('Origin',(0.0262,-0.02545,0.00524999999999988));
#33729=CARTESIAN_POINT('',(0.0211500000000101,-0.02387500000001,0.00525000000000993));
#33730=CARTESIAN_POINT('',(0.0229000000000101,-0.02477500000001,0.00525000000000991));
#33731=CARTESIAN_POINT('Origin',(0.02525,-0.02575,0.00629999999999988));
#33732=CARTESIAN_POINT('',(0.02525,-0.02575,0.00629999999999988));
#33733=CARTESIAN_POINT('',(0.02525,-0.02575,0.00694999999999988));
#33734=CARTESIAN_POINT('',(0.0252500000000101,-0.0257500000000099,0.00630000000000988));
#33735=CARTESIAN_POINT('',(0.02525,-0.02495,0.00629999999999988));
#33736=CARTESIAN_POINT('',(0.0252500000000101,-0.0249250000000099,0.00630000000000988));
#33737=CARTESIAN_POINT('',(0.02525,-0.02495,0.00694999999999988));
#33738=CARTESIAN_POINT('',(0.0252500000000101,-0.02495000000001,0.00630000000000988));
#33739=CARTESIAN_POINT('',(0.0252500000000101,-0.02462500000001,0.00695000000000988));
#33740=CARTESIAN_POINT('Origin',(0.0262,-0.02495,0.00662499999999987));
#33741=CARTESIAN_POINT('',(0.02715,-0.02495,0.00629999999999987));
#33742=CARTESIAN_POINT('',(0.0266750000000101,-0.02495000000001,0.00630000000000997));
#33743=CARTESIAN_POINT('',(0.02715,-0.02495,0.00694999999999987));
#33744=CARTESIAN_POINT('',(0.0271500000000101,-0.02495000000001,-0.000162499999990037));
#33745=CARTESIAN_POINT('',(0.0266750000000101,-0.02495000000001,0.00695000000000997));
#33746=CARTESIAN_POINT('Origin',(0.0262,-0.02575,0.00662499999999987));
#33747=CARTESIAN_POINT('',(0.02715,-0.02575,0.00629999999999987));
#33748=CARTESIAN_POINT('',(0.0266750000000101,-0.0257500000000099,0.00630000000000997));
#33749=CARTESIAN_POINT('',(0.02715,-0.02575,0.00694999999999987));
#33750=CARTESIAN_POINT('',(0.0266750000000101,-0.0257500000000099,0.00695000000000997));
#33751=CARTESIAN_POINT('',(0.0271500000000101,-0.0257500000000099,-0.000162499999990037));
#33752=CARTESIAN_POINT('Origin',(0.02715,-0.0235,0.00694999999999987));
#33753=CARTESIAN_POINT('',(0.02715,-0.0235,0.00694999999999987));
#33754=CARTESIAN_POINT('',(0.0271500000000101,-0.02350000000001,0.00695000000000997));
#33755=CARTESIAN_POINT('',(0.02115,-0.0235,0.00695));
#33756=CARTESIAN_POINT('',(0.0271500000000101,-0.02350000000001,0.00695000000000997));
#33757=CARTESIAN_POINT('',(0.02115,-0.0283,0.00695));
#33758=CARTESIAN_POINT('',(0.02115000000001,-0.02350000000001,0.00695000000000993));
#33759=CARTESIAN_POINT('',(0.02715,-0.0283,0.00694999999999987));
#33760=CARTESIAN_POINT('',(0.0253521645021746,-0.02830000000001,0.00695000000000988));
#33761=CARTESIAN_POINT('',(0.0271500000000101,-0.02350000000001,0.00695000000000997));
#33762=CARTESIAN_POINT('Origin',(0.02715,-0.0235,-0.00695000000000008));
#33763=CARTESIAN_POINT('',(0.02715,-0.0241,0.00629999999999987));
#33764=CARTESIAN_POINT('',(0.0271500000000101,-0.02410000000001,0.00630000000000996));
#33765=CARTESIAN_POINT('',(0.02715,-0.0241,0.00379999999999987));
#33766=CARTESIAN_POINT('',(0.0271500000000101,-0.02410000000001,0.00630000000000996));
#33767=CARTESIAN_POINT('',(0.02715,-0.0235,0.00379999999999987));
#33768=CARTESIAN_POINT('',(0.0271500000000101,-0.0234990000000099,0.00380000000000996));
#33769=CARTESIAN_POINT('',(0.0271500000000101,-0.02350000000001,-0.00694999999999008));
#33770=CARTESIAN_POINT('Origin',(0.0235543290043291,-0.0283,-9.8879238130678E-17));
#33771=CARTESIAN_POINT('',(0.02115,-0.0283,-0.00695));
#33772=CARTESIAN_POINT('',(0.0211500000000101,-0.02830000000001,-0.00587499999999003));
#33773=CARTESIAN_POINT('',(0.02715,-0.0283,-0.00695000000000008));
#33774=CARTESIAN_POINT('',(0.0253521645021746,-0.02830000000001,-0.00694999999999008));
#33775=CARTESIAN_POINT('',(0.0271500000000101,-0.0283000000000099,-0.00347499999999008));
#33776=CARTESIAN_POINT('Origin',(0.02115,-0.0223,-0.01175));
#33777=CARTESIAN_POINT('',(0.02115,-0.0235,0.00629999999999993));
#33778=CARTESIAN_POINT('',(0.0211500000000101,-0.02350000000001,-0.00694999999999007));
#33779=CARTESIAN_POINT('',(0.02115,-0.0241,0.00629999999999993));
#33780=CARTESIAN_POINT('',(0.0211500000000101,-0.02305000000001,0.00630000000000993));
#33781=CARTESIAN_POINT('',(0.02115,-0.0241,0.00529999999999993));
#33782=CARTESIAN_POINT('',(0.0211500000000101,-0.02410000000001,-0.00272499999999003));
#33783=CARTESIAN_POINT('',(0.02115,-0.0235,0.00529999999999993));
#33784=CARTESIAN_POINT('',(0.02115000000001,-0.02305000000001,0.00530000000000993));
#33785=CARTESIAN_POINT('',(0.02115,-0.0235,-0.00530000000000007));
#33786=CARTESIAN_POINT('',(0.0211500000000101,-0.02350000000001,-0.00694999999999007));
#33787=CARTESIAN_POINT('',(0.02115,-0.0241,-0.00530000000000007));
#33788=CARTESIAN_POINT('',(0.02115000000001,-0.02305000000001,-0.00529999999999007));
#33789=CARTESIAN_POINT('',(0.02115,-0.0241,-0.00630000000000007));
#33790=CARTESIAN_POINT('',(0.0211500000000101,-0.02410000000001,-0.00902499999999003));
#33791=CARTESIAN_POINT('',(0.02115,-0.0235,-0.00630000000000007));
#33792=CARTESIAN_POINT('',(0.02115000000001,-0.02305000000001,-0.00629999999999007));
#33793=CARTESIAN_POINT('',(0.02115,-0.0235,-0.00695));
#33794=CARTESIAN_POINT('',(0.0211500000000101,-0.02350000000001,-0.00694999999999007));
#33795=CARTESIAN_POINT('',(0.0211500000000101,-0.02350000000001,-0.00694999999999007));
#33796=CARTESIAN_POINT('Origin',(0.02115,-0.0241,-0.00630000000000007));
#33797=CARTESIAN_POINT('',(0.0229,-0.0241,-0.00530000000000009));
#33798=CARTESIAN_POINT('',(0.0229,-0.0241,-0.00630000000000009));
#33799=CARTESIAN_POINT('',(0.0229000000000101,-0.02410000000001,0.00630000000000991));
#33800=CARTESIAN_POINT('',(0.02515000000001,-0.02410000000001,-0.00629999999999008));
#33801=CARTESIAN_POINT('',(0.0229000000000101,-0.02410000000001,-0.00529999999999007));
#33802=CARTESIAN_POINT('Origin',(0.02515,-0.0241,-0.00630000000000012));
#33803=CARTESIAN_POINT('',(0.02515,-0.0235,-0.00630000000000012));
#33804=CARTESIAN_POINT('',(0.02515,-0.0241,-0.00630000000000012));
#33805=CARTESIAN_POINT('',(0.02515000000001,-0.02350000000001,-0.00629999999999008));
#33806=CARTESIAN_POINT('',(0.02515,-0.0241,-0.00530000000000012));
#33807=CARTESIAN_POINT('',(0.02515000000001,-0.02410000000001,9.88618908959182E-15));
#33808=CARTESIAN_POINT('',(0.02515,-0.0235,-0.00530000000000012));
#33809=CARTESIAN_POINT('',(0.0251500000000101,-0.02350000000001,-0.00529999999999008));
#33810=CARTESIAN_POINT('',(0.02515000000001,-0.02350000000001,-0.00662499999999008));
#33811=CARTESIAN_POINT('Origin',(0.02315,-0.0238,-0.0053000000000001));
#33812=CARTESIAN_POINT('',(0.0251500000000101,-0.02350000000001,-0.00529999999999008));
#33813=CARTESIAN_POINT('',(0.0251500000000101,-0.02410000000001,-0.00529999999999008));
#33814=CARTESIAN_POINT('Origin',(0.02715,-0.0241,0.00629999999999987));
#33815=CARTESIAN_POINT('',(0.02715,-0.0241,-0.00630000000000008));
#33816=CARTESIAN_POINT('',(0.0271500000000101,-0.02410000000001,-0.00629999999999008));
#33817=CARTESIAN_POINT('',(0.02715,-0.0241,-0.00380000000000013));
#33818=CARTESIAN_POINT('',(0.0271500000000101,-0.02410000000001,0.00630000000000996));
#33819=CARTESIAN_POINT('',(0.0229,-0.0241,-0.00380000000000009));
#33820=CARTESIAN_POINT('',(0.0271500000000101,-0.02410000000001,-0.00379999999999007));
#33821=CARTESIAN_POINT('',(0.0229000000000101,-0.02410000000001,0.00630000000000991));
#33822=CARTESIAN_POINT('Origin',(0.02715,-0.0235,-0.00695000000000008));
#33823=CARTESIAN_POINT('',(0.02515000000001,-0.02350000000001,-0.00629999999999008));
#33824=CARTESIAN_POINT('',(0.02515,-0.0235,0.00529999999999989));
#33825=CARTESIAN_POINT('',(0.0251500000000101,-0.02350000000001,0.00530000000000988));
#33826=CARTESIAN_POINT('',(0.02515,-0.0235,0.00629999999999989));
#33827=CARTESIAN_POINT('',(0.0251500000000102,-0.02350000000001,-0.000324999999990115));
#33828=CARTESIAN_POINT('',(0.0251500000000101,-0.02350000000001,0.00630000000000988));
#33829=CARTESIAN_POINT('',(0.0229,-0.0235,0.00379999999999991));
#33830=CARTESIAN_POINT('',(0.0271500000000101,-0.02350000000001,0.00380000000000996));
#33831=CARTESIAN_POINT('',(0.0229,-0.0235,-0.00380000000000009));
#33832=CARTESIAN_POINT('',(0.0229000000000101,-0.02350000000001,-0.00379999999999007));
#33833=CARTESIAN_POINT('',(0.02715,-0.0235,-0.00380000000000013));
#33834=CARTESIAN_POINT('',(0.0271500000000101,-0.02350000000001,-0.00379999999999008));
#33835=CARTESIAN_POINT('',(0.02715,-0.0235,-0.00695000000000008));
#33836=CARTESIAN_POINT('',(0.0271500000000101,-0.02350000000001,-0.00694999999999008));
#33837=CARTESIAN_POINT('',(0.0271500000000101,-0.02350000000001,-0.00694999999999008));
#33838=CARTESIAN_POINT('Origin',(0.02515,-0.0241,0.00629999999999989));
#33839=CARTESIAN_POINT('',(0.0229,-0.0241,0.00629999999999991));
#33840=CARTESIAN_POINT('',(0.0229,-0.0241,0.00529999999999991));
#33841=CARTESIAN_POINT('',(0.0229000000000101,-0.02410000000001,0.00630000000000991));
#33842=CARTESIAN_POINT('',(0.0251500000000101,-0.02410000000001,0.00530000000000988));
#33843=CARTESIAN_POINT('',(0.0251500000000101,-0.02410000000001,0.00630000000000988));
#33844=CARTESIAN_POINT('Origin',(0.02515,-0.0235,0.00629999999999989));
#33845=CARTESIAN_POINT('',(0.02515,-0.0241,0.00629999999999989));
#33846=CARTESIAN_POINT('',(0.0251500000000101,-0.02350000000001,0.00630000000000988));
#33847=CARTESIAN_POINT('',(0.02515,-0.0241,0.00529999999999989));
#33848=CARTESIAN_POINT('',(0.0251500000000101,-0.02350000000001,0.00530000000000988));
#33849=CARTESIAN_POINT('',(0.0251500000000101,-0.02410000000001,0.00630000000000988));
#33850=CARTESIAN_POINT('Origin',(0.02315,-0.0238,0.00529999999999991));
#33851=CARTESIAN_POINT('',(0.0251500000000101,-0.02410000000001,0.00530000000000988));
#33852=CARTESIAN_POINT('Origin',(0.02525,-0.02495,-0.00630000000000012));
#33853=CARTESIAN_POINT('',(0.02525,-0.02495,-0.00695000000000012));
#33854=CARTESIAN_POINT('',(0.02525,-0.02495,-0.00630000000000012));
#33855=CARTESIAN_POINT('',(0.0252500000000101,-0.02495000000001,-0.00694999999999008));
#33856=CARTESIAN_POINT('',(0.02525,-0.02575,-0.00630000000000012));
#33857=CARTESIAN_POINT('',(0.0252500000000101,-0.02452500000001,-0.00629999999999008));
#33858=CARTESIAN_POINT('',(0.02525,-0.02575,-0.00695000000000012));
#33859=CARTESIAN_POINT('',(0.0252500000000101,-0.0257500000000099,-0.00694999999999008));
#33860=CARTESIAN_POINT('',(0.0252500000000101,-0.02422500000001,-0.00694999999999008));
#33861=CARTESIAN_POINT('Origin',(0.0262,-0.02495,-0.00662500000000013));
#33862=CARTESIAN_POINT('',(0.02715,-0.02495,-0.00695000000000008));
#33863=CARTESIAN_POINT('',(0.0266750000000101,-0.02495000000001,-0.00694999999999007));
#33864=CARTESIAN_POINT('',(0.02715,-0.02495,-0.00630000000000008));
#33865=CARTESIAN_POINT('',(0.0271500000000101,-0.02495000000001,-0.00678749999999008));
#33866=CARTESIAN_POINT('',(0.0266750000000101,-0.02495000000001,-0.00629999999999007));
#33867=CARTESIAN_POINT('Origin',(0.0262,-0.02575,-0.00662500000000013));
#33868=CARTESIAN_POINT('',(0.02715,-0.02575,-0.00695000000000008));
#33869=CARTESIAN_POINT('',(0.0266750000000101,-0.0257500000000099,-0.00694999999999007));
#33870=CARTESIAN_POINT('',(0.02715,-0.02575,-0.00630000000000008));
#33871=CARTESIAN_POINT('',(0.0266750000000101,-0.0257500000000099,-0.00629999999999007));
#33872=CARTESIAN_POINT('',(0.0271500000000101,-0.0257500000000099,-0.00678749999999008));
#33873=CARTESIAN_POINT('Origin',(0.02715,-0.0235,-0.00695000000000008));
#33874=CARTESIAN_POINT('',(0.0271500000000101,-0.02350000000001,-0.00694999999999008));
#33875=CARTESIAN_POINT('',(0.02715,-0.0276,-0.00630000000000008));
#33876=CARTESIAN_POINT('',(0.0271500000000101,-0.02410000000001,-0.00629999999999008));
#33877=CARTESIAN_POINT('',(0.02715,-0.0276,0.00629999999999987));
#33878=CARTESIAN_POINT('',(0.0271500000000101,-0.0276000000000099,0.00630000000000996));
#33879=CARTESIAN_POINT('',(0.0271500000000101,-0.02410000000001,0.00630000000000996));
#33880=CARTESIAN_POINT('Origin',(0.02715,-0.0235,-0.00695000000000008));
#33881=CARTESIAN_POINT('',(0.0271500000000101,-0.02350000000001,-0.00694999999999008));
#33882=CARTESIAN_POINT('',(0.0271500000000101,-0.0234990000000099,-0.00379999999999008));
#33883=CARTESIAN_POINT('',(0.0271500000000101,-0.02410000000001,-0.00629999999999008));
#33884=CARTESIAN_POINT('Origin',(0.02715,-0.0235,-0.00695000000000008));
#33885=CARTESIAN_POINT('Origin',(0.02715,-0.023499,-0.00380000000000013));
#33886=CARTESIAN_POINT('',(0.0229000000000101,-0.02349900000001,-0.00379999999999007));
#33887=CARTESIAN_POINT('Origin',(0.02715,-0.0241,-0.00630000000000008));
#33888=CARTESIAN_POINT('',(0.0229,-0.02575,-0.00630000000000009));
#33889=CARTESIAN_POINT('',(0.0229000000000101,-0.02410000000001,-0.00629999999999007));
#33890=CARTESIAN_POINT('',(0.0223,-0.02635,-0.00630000000000009));
#33891=CARTESIAN_POINT('',(0.0229000000000101,-0.02575000000001,-0.00629999999999007));
#33892=CARTESIAN_POINT('',(0.0223,-0.0276,-0.00630000000000009));
#33893=CARTESIAN_POINT('',(0.0223000000000101,-0.0263500000000099,-0.00629999999999008));
#33894=CARTESIAN_POINT('',(0.0271500000000101,-0.0276000000000099,-0.00629999999999008));
#33895=CARTESIAN_POINT('Origin',(0.02715,-0.0276,0.00629999999999987));
#33896=CARTESIAN_POINT('',(0.0223,-0.0276,0.00629999999999991));
#33897=CARTESIAN_POINT('',(0.0223000000000101,-0.0276000000000099,0.00630000000000991));
#33898=CARTESIAN_POINT('',(0.0271500000000101,-0.0276000000000099,0.00630000000000996));
#33899=CARTESIAN_POINT('Origin',(0.02715,-0.0241,0.00629999999999987));
#33900=CARTESIAN_POINT('',(0.0223,-0.02635,0.00629999999999991));
#33901=CARTESIAN_POINT('',(0.0223000000000101,-0.0263500000000099,0.00630000000000991));
#33902=CARTESIAN_POINT('',(0.0229,-0.02575,0.00629999999999991));
#33903=CARTESIAN_POINT('',(0.0229000000000101,-0.02575000000001,0.00630000000000991));
#33904=CARTESIAN_POINT('',(0.0229000000000101,-0.02410000000001,0.00630000000000991));
#33905=CARTESIAN_POINT('',(0.0271500000000101,-0.02410000000001,0.00630000000000996));
#33906=CARTESIAN_POINT('Origin',(0.02715,-0.0241,0.00629999999999987));
#33907=CARTESIAN_POINT('',(0.0229,-0.0241,0.00379999999999991));
#33908=CARTESIAN_POINT('',(0.0229000000000101,-0.02410000000001,0.00630000000000991));
#33909=CARTESIAN_POINT('',(0.0271500000000101,-0.02410000000001,0.00380000000000996));
#33910=CARTESIAN_POINT('Origin',(0.02715,-0.023499,0.00379999999999987));
#33911=CARTESIAN_POINT('',(0.0229000000000101,-0.02349900000001,0.00380000000000991));
#33912=CARTESIAN_POINT('Origin',(0.0229,-0.0241,0.00629999999999991));
#33913=CARTESIAN_POINT('',(0.0229000000000101,-0.02575000000001,0.00630000000000991));
#33914=CARTESIAN_POINT('Origin',(0.0229,-0.02575,0.00629999999999991));
#33915=CARTESIAN_POINT('',(0.0223000000000101,-0.0263500000000099,0.00630000000000991));
#33916=CARTESIAN_POINT('Origin',(0.0223,-0.02635,0.00629999999999991));
#33917=CARTESIAN_POINT('',(0.,0.,0.));
#33918=CARTESIAN_POINT('Origin',(-4.42567805516485E-17,-0.017,1.23897393496637E-32));
#33919=CARTESIAN_POINT('',(-0.000529682692573584,-0.01700000000001,0.0024432429771081));
#33920=CARTESIAN_POINT('Origin',(-4.42567805516478E-17,-0.01700000000001,
1.23897393496654E-32));
#33921=CARTESIAN_POINT('',(-0.000529682692573584,-0.01550000000001,0.0024432429771081));
#33922=CARTESIAN_POINT('',(-0.000529682692573584,-0.017,0.0024432429771081));
#33923=CARTESIAN_POINT('Origin',(-4.43566503645865E-17,-0.01550000000001,
1.21332054810731E-32));
#33924=CARTESIAN_POINT('Origin',(5.68609676360377E-5,-0.017,-2.15928534185712E-5));
#33925=CARTESIAN_POINT('',(0.00259933789198903,-0.01550000000001,-0.0117491591435374));
#33926=CARTESIAN_POINT('Origin',(5.68609676479293E-5,-0.01550000000001,
-2.15928534262255E-5));
#33927=CARTESIAN_POINT('',(0.00259933789198903,-0.01700000000001,-0.0117491591435374));
#33928=CARTESIAN_POINT('',(0.00259933789198903,-0.017,-0.0117491591435374));
#33929=CARTESIAN_POINT('Origin',(5.68609676479294E-5,-0.01700000000001,
-2.15928534262255E-5));
#33930=CARTESIAN_POINT('Origin',(5.68609676360372E-5,-0.017,-2.15928534185708E-5));
#33931=CARTESIAN_POINT('Origin',(5.68609676360371E-5,-0.0155,-2.15928534185708E-5));
#33932=CARTESIAN_POINT('',(0.,0.,0.));
#33933=CARTESIAN_POINT('Origin',(0.00643329000430773,-0.008,0.0115261780187742));
#33934=CARTESIAN_POINT('',(0.00621272270841098,-0.008,0.011643864330556));
#33935=CARTESIAN_POINT('',(0.00655513261802568,-0.008,0.0117444768448874));
#33936=CARTESIAN_POINT('Origin',(0.00643329000431773,-0.00799999999999,
0.0115261780187842));
#33937=CARTESIAN_POINT('',(0.00655513261802568,-0.024,0.0117444768448874));
#33938=CARTESIAN_POINT('',(0.00655513261803568,-0.00799999999999,0.0117444768448974));
#33939=CARTESIAN_POINT('',(0.00621272270841098,-0.024,0.011643864330556));
#33940=CARTESIAN_POINT('Origin',(0.00643329000431773,-0.02400000000001,
0.0115261780187842));
#33941=CARTESIAN_POINT('',(0.00621272270842098,-0.00799999999999,0.011643864330566));
#33942=CARTESIAN_POINT('Origin',(-4.44089209850063E-17,-0.008,6.72997231505748E-33));
#33943=CARTESIAN_POINT('',(0.00689344899281767,-0.008,0.0115491497948299));
#33944=CARTESIAN_POINT('Origin',(-4.44089209850063E-17,-0.00799999999999,
6.72997231505748E-33));
#33945=CARTESIAN_POINT('',(0.00689344899281767,-0.024,0.0115491497948299));
#33946=CARTESIAN_POINT('',(0.00689344899282767,-0.00799999999999,0.0115491497948399));
#33947=CARTESIAN_POINT('Origin',(-4.44089209850063E-17,-0.02400000000001,
6.72997231505748E-33));
#33948=CARTESIAN_POINT('Origin',(0.00676531797064634,-0.008,0.0113344815830301));
#33949=CARTESIAN_POINT('',(0.00697752095427542,-0.008,0.0112023078574304));
#33950=CARTESIAN_POINT('Origin',(0.00676531797065634,-0.00799999999999,
0.0113344815830401));
#33951=CARTESIAN_POINT('',(0.00697752095427542,-0.024,0.0112023078574304));
#33952=CARTESIAN_POINT('',(0.00697752095428542,-0.00799999999999,0.0112023078574404));
#33953=CARTESIAN_POINT('Origin',(0.00676531797065634,-0.02400000000001,
0.0113344815830401));
#33954=CARTESIAN_POINT('Origin',(0.00687303373118604,-0.008,0.0110345551487125));
#33955=CARTESIAN_POINT('',(0.00687303373118604,-0.008,0.0110345551487125));
#33956=CARTESIAN_POINT('',(0.00673974017575285,-0.00799999999999,0.0108205542946554));
#33957=CARTESIAN_POINT('',(0.00687303373118604,-0.024,0.0110345551487125));
#33958=CARTESIAN_POINT('',(0.00687303373119603,-0.016,0.0110345551487225));
#33959=CARTESIAN_POINT('',(0.00673974017575285,-0.02400000000001,0.0108205542946554));
#33960=CARTESIAN_POINT('Origin',(0.00788272044413945,-0.008,0.0105878571202838));
#33961=CARTESIAN_POINT('',(0.00767940127818881,-0.008,0.0107333264186156));
#33962=CARTESIAN_POINT('',(0.00803201439194512,-0.008,0.0107883847172589));
#33963=CARTESIAN_POINT('Origin',(0.00788272044414944,-0.00799999999999,
0.0105878571202938));
#33964=CARTESIAN_POINT('',(0.00803201439194512,-0.024,0.0107883847172589));
#33965=CARTESIAN_POINT('',(0.00803201439195513,-0.00799999999999,0.0107883847172689));
#33966=CARTESIAN_POINT('',(0.00767940127818881,-0.024,0.0107333264186156));
#33967=CARTESIAN_POINT('Origin',(0.00788272044414944,-0.02400000000001,
0.0105878571202938));
#33968=CARTESIAN_POINT('',(0.00767940127819881,-0.00799999999999,0.0107333264186256));
#33969=CARTESIAN_POINT('Origin',(-4.44089209850063E-17,-0.008,6.72997231505748E-33));
#33970=CARTESIAN_POINT('',(0.00834194112716969,-0.008,0.0105505695690249));
#33971=CARTESIAN_POINT('Origin',(-4.44089209850063E-17,-0.00799999999999,
6.72997231505748E-33));
#33972=CARTESIAN_POINT('',(0.00834194112716969,-0.024,0.0105505695690249));
#33973=CARTESIAN_POINT('',(0.00834194112717969,-0.00799999999999,0.0105505695690349));
#33974=CARTESIAN_POINT('Origin',(-4.44089209850063E-17,-0.02400000000001,
6.72997231505748E-33));
#33975=CARTESIAN_POINT('Origin',(0.00818688645937843,-0.008,0.010354462327965));
#33976=CARTESIAN_POINT('',(0.0083800218839516,-0.008,0.0101957213194796));
#33977=CARTESIAN_POINT('Origin',(0.00818688645938842,-0.00799999999999,
0.010354462327975));
#33978=CARTESIAN_POINT('',(0.0083800218839516,-0.024,0.0101957213194796));
#33979=CARTESIAN_POINT('',(0.00838002188396161,-0.00799999999999,0.0101957213194896));
#33980=CARTESIAN_POINT('Origin',(0.00818688645938842,-0.02400000000001,
0.010354462327975));
#33981=CARTESIAN_POINT('Origin',(0.00825453244123688,-0.008,0.0100430420778053));
#33982=CARTESIAN_POINT('',(0.00825453244123688,-0.008,0.0100430420778053));
#33983=CARTESIAN_POINT('',(0.00818084247458016,-0.00799999999999,0.0099533857052449));
#33984=CARTESIAN_POINT('',(0.00825453244123688,-0.024,0.0100430420778053));
#33985=CARTESIAN_POINT('',(0.00825453244124687,-0.016,0.0100430420778153));
#33986=CARTESIAN_POINT('',(0.00818084247458016,-0.02400000000001,0.0099533857052449));
#33987=CARTESIAN_POINT('Origin',(0.00919727535166895,-0.008,0.00946837505095685));
#33988=CARTESIAN_POINT('',(0.00901468316296453,-0.008,0.00963913831581242));
#33989=CARTESIAN_POINT('',(0.00937146617272329,-0.008,0.00964770033601285));
#33990=CARTESIAN_POINT('Origin',(0.00919727535167895,-0.00799999999999,
0.00946837505096685));
#33991=CARTESIAN_POINT('',(0.00937146617272329,-0.024,0.00964770033601285));
#33992=CARTESIAN_POINT('',(0.00937146617273328,-0.00799999999999,0.00964770033602285));
#33993=CARTESIAN_POINT('',(0.00901468316296453,-0.024,0.00963913831581242));
#33994=CARTESIAN_POINT('Origin',(0.00919727535167895,-0.02400000000001,
0.00946837505096685));
#33995=CARTESIAN_POINT('',(0.00901468316297454,-0.00799999999999,0.00963913831582242));
#33996=CARTESIAN_POINT('Origin',(-4.44089209850063E-17,-0.008,6.72997231505748E-33));
#33997=CARTESIAN_POINT('',(0.0096477003360128,-0.008,0.00937146617272333));
#33998=CARTESIAN_POINT('Origin',(-4.44089209850063E-17,-0.00799999999999,
6.72997231505748E-33));
#33999=CARTESIAN_POINT('',(0.0096477003360128,-0.024,0.00937146617272333));
#34000=CARTESIAN_POINT('',(0.00964770033602281,-0.00799999999999,0.00937146617273333));
#34001=CARTESIAN_POINT('Origin',(-4.44089209850063E-17,-0.02400000000001,
6.72997231505748E-33));
#34002=CARTESIAN_POINT('Origin',(0.0094683750509568,-0.008,0.00919727535166899));
#34003=CARTESIAN_POINT('',(0.00963913831581237,-0.008,0.00901468316296458));
#34004=CARTESIAN_POINT('Origin',(0.0094683750509668,-0.00799999999999,0.00919727535167899));
#34005=CARTESIAN_POINT('',(0.00963913831581237,-0.024,0.00901468316296458));
#34006=CARTESIAN_POINT('',(0.00963913831582238,-0.00799999999999,0.00901468316297458));
#34007=CARTESIAN_POINT('Origin',(0.0094683750509668,-0.02400000000001,0.00919727535167899));
#34008=CARTESIAN_POINT('Origin',(0.00949479381262939,-0.008,0.00887968977248946));
#34009=CARTESIAN_POINT('',(0.00949479381262939,-0.008,0.00887968977248946));
#34010=CARTESIAN_POINT('',(0.00942962993438202,-0.00799999999999,0.00881874742507027));
#34011=CARTESIAN_POINT('',(0.00949479381262939,-0.024,0.00887968977248946));
#34012=CARTESIAN_POINT('',(0.00949479381263939,-0.016,0.00887968977249946));
#34013=CARTESIAN_POINT('',(0.00942962993438202,-0.02400000000001,0.00881874742507027));
#34014=CARTESIAN_POINT('Origin',(0.010354462327965,-0.008,0.00818688645937847));
#34015=CARTESIAN_POINT('',(0.0101957213194795,-0.008,0.00838002188395165));
#34016=CARTESIAN_POINT('',(0.0105505695690249,-0.008,0.00834194112716973));
#34017=CARTESIAN_POINT('Origin',(0.010354462327975,-0.00799999999999,0.00818688645938847));
#34018=CARTESIAN_POINT('',(0.0105505695690249,-0.024,0.00834194112716973));
#34019=CARTESIAN_POINT('',(0.0105505695690349,-0.00799999999999,0.00834194112717973));
#34020=CARTESIAN_POINT('',(0.0101957213194795,-0.024,0.00838002188395165));
#34021=CARTESIAN_POINT('Origin',(0.010354462327975,-0.02400000000001,0.00818688645938847));
#34022=CARTESIAN_POINT('',(0.0101957213194895,-0.00799999999999,0.00838002188396165));
#34023=CARTESIAN_POINT('Origin',(-4.44089209850063E-17,-0.008,6.72997231505748E-33));
#34024=CARTESIAN_POINT('',(0.0107883847172589,-0.008,0.00803201439194517));
#34025=CARTESIAN_POINT('Origin',(-4.44089209850063E-17,-0.00799999999999,
6.72997231505748E-33));
#34026=CARTESIAN_POINT('',(0.0107883847172589,-0.024,0.00803201439194517));
#34027=CARTESIAN_POINT('',(0.0107883847172689,-0.00799999999999,0.00803201439195516));
#34028=CARTESIAN_POINT('Origin',(-4.44089209850063E-17,-0.02400000000001,
6.72997231505748E-33));
#34029=CARTESIAN_POINT('Origin',(0.0105878571202839,-0.008,0.00788272044413949));
#34030=CARTESIAN_POINT('',(0.0107333264186156,-0.008,0.00767940127818885));
#34031=CARTESIAN_POINT('Origin',(0.0105878571202939,-0.00799999999999,0.00788272044414949));
#34032=CARTESIAN_POINT('',(0.0107333264186156,-0.024,0.00767940127818885));
#34033=CARTESIAN_POINT('',(0.0107333264186256,-0.00799999999999,0.00767940127819885));
#34034=CARTESIAN_POINT('Origin',(0.0105878571202939,-0.02400000000001,0.00788272044414949));
#34035=CARTESIAN_POINT('Origin',(0.0105725966294337,-0.008,0.00756440351325123));
#34036=CARTESIAN_POINT('',(0.0105725966294337,-0.008,0.00756440351325123));
#34037=CARTESIAN_POINT('',(0.0104326500269425,-0.00799999999999,0.00746427554955177));
#34038=CARTESIAN_POINT('',(0.0105725966294337,-0.024,0.00756440351325123));
#34039=CARTESIAN_POINT('',(0.0105725966294436,-0.016,0.00756440351326123));
#34040=CARTESIAN_POINT('',(0.0104326500269425,-0.02400000000001,0.00746427554955177));
#34041=CARTESIAN_POINT('Origin',(0.0113344815830301,-0.008,0.00676531797064638));
#34042=CARTESIAN_POINT('',(0.0112023078574304,-0.008,0.00697752095427547));
#34043=CARTESIAN_POINT('',(0.0115491497948299,-0.008,0.00689344899281771));
#34044=CARTESIAN_POINT('Origin',(0.0113344815830401,-0.00799999999999,0.00676531797065638));
#34045=CARTESIAN_POINT('',(0.0115491497948299,-0.024,0.00689344899281771));
#34046=CARTESIAN_POINT('',(0.0115491497948398,-0.00799999999999,0.00689344899282771));
#34047=CARTESIAN_POINT('',(0.0112023078574304,-0.024,0.00697752095427547));
#34048=CARTESIAN_POINT('Origin',(0.0113344815830401,-0.02400000000001,0.00676531797065638));
#34049=CARTESIAN_POINT('',(0.0112023078574404,-0.00799999999999,0.00697752095428547));
#34050=CARTESIAN_POINT('Origin',(-4.44089209850063E-17,-0.008,6.72997231505748E-33));
#34051=CARTESIAN_POINT('',(0.0117444768448874,-0.008,0.00655513261802572));
#34052=CARTESIAN_POINT('Origin',(-4.44089209850063E-17,-0.00799999999999,
6.72997231505748E-33));
#34053=CARTESIAN_POINT('',(0.0117444768448874,-0.024,0.00655513261802572));
#34054=CARTESIAN_POINT('',(0.0117444768448974,-0.00799999999999,0.00655513261803572));
#34055=CARTESIAN_POINT('Origin',(-4.44089209850063E-17,-0.02400000000001,
6.72997231505748E-33));
#34056=CARTESIAN_POINT('Origin',(0.0115261780187742,-0.008,0.00643329000430777));
#34057=CARTESIAN_POINT('',(0.011643864330556,-0.008,0.00621272270841103));
#34058=CARTESIAN_POINT('Origin',(0.0115261780187842,-0.00799999999999,0.00643329000431777));
#34059=CARTESIAN_POINT('',(0.011643864330556,-0.024,0.00621272270841103));
#34060=CARTESIAN_POINT('',(0.011643864330566,-0.00799999999999,0.00621272270842103));
#34061=CARTESIAN_POINT('Origin',(0.0115261780187842,-0.02400000000001,0.00643329000431777));
#34062=CARTESIAN_POINT('Origin',(0.0114694993866308,-0.008,0.0061196882126524));
#34063=CARTESIAN_POINT('',(0.0114694993866308,-0.008,0.0061196882126524));
#34064=CARTESIAN_POINT('',(0.0111490530784194,-0.00799999999999,0.00594871026243939));
#34065=CARTESIAN_POINT('',(0.0114694993866308,-0.024,0.0061196882126524));
#34066=CARTESIAN_POINT('',(0.0114694993866408,-0.016,0.0061196882126624));
#34067=CARTESIAN_POINT('',(0.0111490530784194,-0.02400000000001,0.00594871026243939));
#34068=CARTESIAN_POINT('Origin',(0.0114165205192449,-0.008,0.00711094643726559));
#34069=CARTESIAN_POINT('',(0.0110345551487124,-0.024,0.00687303373118608));
#34070=CARTESIAN_POINT('',(0.0110115369799215,-0.02400000000001,0.00685869652879265));
#34071=CARTESIAN_POINT('',(0.0110345551487124,-0.008,0.00687303373118608));
#34072=CARTESIAN_POINT('',(0.0110345551487224,-0.016,0.00687303373119607));
#34073=CARTESIAN_POINT('',(0.0110115369799215,-0.00799999999999,0.00685869652879265));
#34074=CARTESIAN_POINT('Origin',(0.010390685842037,-0.008,0.0085402662565105));
#34075=CARTESIAN_POINT('',(0.0100430420778052,-0.024,0.00825453244123691));
#34076=CARTESIAN_POINT('',(0.0101272075873608,-0.02400000000001,0.008323709382217));
#34077=CARTESIAN_POINT('',(0.0100430420778052,-0.008,0.00825453244123691));
#34078=CARTESIAN_POINT('',(0.0100430420778153,-0.016,0.00825453244124691));
#34079=CARTESIAN_POINT('',(0.0101272075873608,-0.00799999999999,0.008323709382217));
#34080=CARTESIAN_POINT('Origin',(0.00782624825024835,-0.008,0.0109385711281449));
#34081=CARTESIAN_POINT('',(0.00756440351325119,-0.024,0.0105725966294337));
#34082=CARTESIAN_POINT('',(0.00759519791805031,-0.02400000000001,0.0106156372762982));
#34083=CARTESIAN_POINT('',(0.00756440351325119,-0.008,0.0105725966294337));
#34084=CARTESIAN_POINT('',(0.00756440351326119,-0.016,0.0105725966294437));
#34085=CARTESIAN_POINT('',(0.00759519791805031,-0.00799999999999,0.0106156372762982));
#34086=CARTESIAN_POINT('Origin',(0.00633152357385956,-0.008,0.0118665205192449));
#34087=CARTESIAN_POINT('',(0.00611968821265236,-0.024,0.0114694993866308));
#34088=CARTESIAN_POINT('',(0.00605462794304295,-0.02400000000001,0.0113475636447265));
#34089=CARTESIAN_POINT('',(0.00611968821265236,-0.008,0.0114694993866308));
#34090=CARTESIAN_POINT('',(0.00611968821266236,-0.016,0.0114694993866408));
#34091=CARTESIAN_POINT('',(0.00605462794304295,-0.00799999999999,0.0113475636447265));
#34092=CARTESIAN_POINT('Origin',(-4.44089209850063E-17,-0.016,6.72997231505748E-33));
#34093=CARTESIAN_POINT('',(0.0117336086965482,-0.008,0.00559664425850784));
#34094=CARTESIAN_POINT('Origin',(-4.44089209850063E-17,-0.00799999999999,
6.72997231505748E-33));
#34095=CARTESIAN_POINT('',(0.0117336086965482,-0.024,0.00559664425850784));
#34096=CARTESIAN_POINT('',(0.0117336086965582,-0.016,0.00559664425851784));
#34097=CARTESIAN_POINT('Origin',(-4.44089209850063E-17,-0.02400000000001,
6.72997231505748E-33));
#34098=CARTESIAN_POINT('Origin',(-4.44089209850063E-17,-0.016,6.72997231505748E-33));
#34099=CARTESIAN_POINT('Origin',(-4.44089209850063E-17,-0.02400000000001,
6.72997231505748E-33));
#34100=CARTESIAN_POINT('Origin',(-4.44089209850063E-17,-0.00799999999999,
6.72997231505748E-33));
#34101=CARTESIAN_POINT('Origin',(0.00907128985548541,-0.024,0.00907128985548545));
#34102=CARTESIAN_POINT('',(0.0125459354524631,-0.024,0.0059841042456353));
#34103=CARTESIAN_POINT('',(0.0125459354524731,-0.02400000000001,0.0059841042456453));
#34104=CARTESIAN_POINT('',(0.00598410424563526,-0.024,0.0125459354524631));
#34105=CARTESIAN_POINT('Origin',(-4.44089209850063E-17,-0.02400000000001,
6.72997231505748E-33));
#34106=CARTESIAN_POINT('',(0.0055966442585078,-0.024,0.0117336086965482));
#34107=CARTESIAN_POINT('',(0.0055966442585178,-0.02400000000001,0.0117336086965582));
#34108=CARTESIAN_POINT('Origin',(-4.44089209850063E-17,-0.02400000000001,
6.72997231505748E-33));
#34109=CARTESIAN_POINT('Origin',(-4.44089209850063E-17,-0.02400000000001,
6.72997231505748E-33));
#34110=CARTESIAN_POINT('',(0.00887968977248941,-0.024,0.00949479381262943));
#34111=CARTESIAN_POINT('Origin',(-4.44089209850063E-17,-0.02400000000001,
6.72997231505748E-33));
#34112=CARTESIAN_POINT('',(0.00897243436344023,-0.02400000000001,0.00959396290421603));
#34113=CARTESIAN_POINT('Origin',(-4.44089209850063E-17,-0.02400000000001,
6.72997231505748E-33));
#34114=CARTESIAN_POINT('Origin',(-4.44089209850063E-17,-0.016,6.72997231505748E-33));
#34115=CARTESIAN_POINT('',(0.00887968977248941,-0.008,0.00949479381262943));
#34116=CARTESIAN_POINT('Origin',(-4.44089209850063E-17,-0.00799999999999,
6.72997231505748E-33));
#34117=CARTESIAN_POINT('',(0.00887968977249942,-0.016,0.00949479381263943));
#34118=CARTESIAN_POINT('Origin',(-4.44089209850063E-17,-0.016,6.72997231505748E-33));
#34119=CARTESIAN_POINT('',(0.0055966442585078,-0.008,0.0117336086965482));
#34120=CARTESIAN_POINT('',(0.0055966442585178,-0.016,0.0117336086965582));
#34121=CARTESIAN_POINT('Origin',(-4.44089209850063E-17,-0.00799999999999,
6.72997231505748E-33));
#34122=CARTESIAN_POINT('Origin',(0.00918706364922943,-0.008,0.00982345975229737));
#34123=CARTESIAN_POINT('',(0.00897243436344023,-0.00799999999999,0.00959396290421603));
#34124=CARTESIAN_POINT('Origin',(-4.44089209850063E-17,-0.016,6.72997231505748E-33));
#34125=CARTESIAN_POINT('Origin',(-4.44089209850063E-17,-0.00799999999999,
6.72997231505748E-33));
#34126=CARTESIAN_POINT('Origin',(0.0125459354524631,-0.016,0.0059841042456353));
#34127=CARTESIAN_POINT('',(0.0125459354524631,-0.008,0.0059841042456353));
#34128=CARTESIAN_POINT('',(0.0125459354524731,-0.00799999999999,0.0059841042456453));
#34129=CARTESIAN_POINT('',(0.0125459354524731,-0.016,0.0059841042456453));
#34130=CARTESIAN_POINT('Origin',(-4.44089209850063E-17,-0.016,6.72997231505748E-33));
#34131=CARTESIAN_POINT('',(0.00598410424563526,-0.008,0.0125459354524631));
#34132=CARTESIAN_POINT('Origin',(-4.44089209850063E-17,-0.00799999999999,
6.72997231505748E-33));
#34133=CARTESIAN_POINT('',(0.00598410424564526,-0.016,0.0125459354524731));
#34134=CARTESIAN_POINT('Origin',(0.0055966442585078,-0.016,0.0117336086965482));
#34135=CARTESIAN_POINT('',(0.0055966442585178,-0.00799999999999,0.0117336086965582));
#34136=CARTESIAN_POINT('Origin',(-4.44089209850063E-17,-0.016,6.72997231505748E-33));
#34137=CARTESIAN_POINT('Origin',(-4.44089209850063E-17,-0.00799999999999,
6.72997231505748E-33));
#34138=CARTESIAN_POINT('Origin',(0.00907128985548541,-0.008,0.00907128985548545));
#34139=CARTESIAN_POINT('',(0.,0.,0.));
#34140=CARTESIAN_POINT('Origin',(-0.0115261780187742,-0.008,0.00643329000430777));
#34141=CARTESIAN_POINT('',(-0.011643864330556,-0.008,0.00621272270841102));
#34142=CARTESIAN_POINT('',(-0.0117444768448874,-0.008,0.00655513261802572));
#34143=CARTESIAN_POINT('Origin',(-0.0115261780187842,-0.00799999999999,
0.00643329000431777));
#34144=CARTESIAN_POINT('',(-0.0117444768448874,-0.024,0.00655513261802572));
#34145=CARTESIAN_POINT('',(-0.0117444768448974,-0.00799999999999,0.00655513261803572));
#34146=CARTESIAN_POINT('',(-0.011643864330556,-0.024,0.00621272270841102));
#34147=CARTESIAN_POINT('Origin',(-0.0115261780187842,-0.02400000000001,
0.00643329000431777));
#34148=CARTESIAN_POINT('',(-0.011643864330566,-0.00799999999999,0.00621272270842102));
#34149=CARTESIAN_POINT('Origin',(-4.44089209850063E-17,-0.008,6.72997231505748E-33));
#34150=CARTESIAN_POINT('',(-0.0115491497948299,-0.008,0.00689344899281771));
#34151=CARTESIAN_POINT('Origin',(-4.44089209850063E-17,-0.00799999999999,
6.72997231505748E-33));
#34152=CARTESIAN_POINT('',(-0.0115491497948299,-0.024,0.00689344899281771));
#34153=CARTESIAN_POINT('',(-0.0115491497948399,-0.00799999999999,0.00689344899282771));
#34154=CARTESIAN_POINT('Origin',(-4.44089209850063E-17,-0.02400000000001,
6.72997231505748E-33));
#34155=CARTESIAN_POINT('Origin',(-0.0113344815830301,-0.008,0.00676531797064638));
#34156=CARTESIAN_POINT('',(-0.0112023078574304,-0.008,0.00697752095427546));
#34157=CARTESIAN_POINT('Origin',(-0.0113344815830401,-0.00799999999999,
0.00676531797065638));
#34158=CARTESIAN_POINT('',(-0.0112023078574304,-0.024,0.00697752095427546));
#34159=CARTESIAN_POINT('',(-0.0112023078574404,-0.00799999999999,0.00697752095428546));
#34160=CARTESIAN_POINT('Origin',(-0.0113344815830401,-0.02400000000001,
0.00676531797065638));
#34161=CARTESIAN_POINT('Origin',(-0.0110345551487125,-0.008,0.00687303373118608));
#34162=CARTESIAN_POINT('',(-0.0110345551487125,-0.008,0.00687303373118608));
#34163=CARTESIAN_POINT('',(-0.0108205542946554,-0.00799999999999,0.00673974017575289));
#34164=CARTESIAN_POINT('',(-0.0110345551487125,-0.024,0.00687303373118608));
#34165=CARTESIAN_POINT('',(-0.0110345551487225,-0.016,0.00687303373119607));
#34166=CARTESIAN_POINT('',(-0.0108205542946554,-0.02400000000001,0.00673974017575289));
#34167=CARTESIAN_POINT('Origin',(-0.0105878571202838,-0.008,0.00788272044413949));
#34168=CARTESIAN_POINT('',(-0.0107333264186156,-0.008,0.00767940127818885));
#34169=CARTESIAN_POINT('',(-0.0107883847172589,-0.008,0.00803201439194517));
#34170=CARTESIAN_POINT('Origin',(-0.0105878571202938,-0.00799999999999,
0.00788272044414949));
#34171=CARTESIAN_POINT('',(-0.0107883847172589,-0.024,0.00803201439194517));
#34172=CARTESIAN_POINT('',(-0.0107883847172689,-0.00799999999999,0.00803201439195517));
#34173=CARTESIAN_POINT('',(-0.0107333264186156,-0.024,0.00767940127818885));
#34174=CARTESIAN_POINT('Origin',(-0.0105878571202938,-0.02400000000001,
0.00788272044414949));
#34175=CARTESIAN_POINT('',(-0.0107333264186256,-0.00799999999999,0.00767940127819885));
#34176=CARTESIAN_POINT('Origin',(-4.44089209850063E-17,-0.008,6.72997231505748E-33));
#34177=CARTESIAN_POINT('',(-0.0105505695690249,-0.008,0.00834194112716973));
#34178=CARTESIAN_POINT('Origin',(-4.44089209850063E-17,-0.00799999999999,
6.72997231505748E-33));
#34179=CARTESIAN_POINT('',(-0.0105505695690249,-0.024,0.00834194112716973));
#34180=CARTESIAN_POINT('',(-0.0105505695690349,-0.00799999999999,0.00834194112717973));
#34181=CARTESIAN_POINT('Origin',(-4.44089209850063E-17,-0.02400000000001,
6.72997231505748E-33));
#34182=CARTESIAN_POINT('Origin',(-0.010354462327965,-0.008,0.00818688645937847));
#34183=CARTESIAN_POINT('',(-0.0101957213194796,-0.008,0.00838002188395165));
#34184=CARTESIAN_POINT('Origin',(-0.010354462327975,-0.00799999999999,0.00818688645938847));
#34185=CARTESIAN_POINT('',(-0.0101957213194796,-0.024,0.00838002188395165));
#34186=CARTESIAN_POINT('',(-0.0101957213194896,-0.00799999999999,0.00838002188396165));
#34187=CARTESIAN_POINT('Origin',(-0.010354462327975,-0.02400000000001,0.00818688645938847));
#34188=CARTESIAN_POINT('Origin',(-0.0100430420778053,-0.008,0.00825453244123692));
#34189=CARTESIAN_POINT('',(-0.0100430420778053,-0.008,0.00825453244123692));
#34190=CARTESIAN_POINT('',(-0.00995338570524494,-0.00799999999999,0.00818084247458021));
#34191=CARTESIAN_POINT('',(-0.0100430420778053,-0.024,0.00825453244123692));
#34192=CARTESIAN_POINT('',(-0.0100430420778153,-0.016,0.00825453244124691));
#34193=CARTESIAN_POINT('',(-0.00995338570524494,-0.02400000000001,0.00818084247458021));
#34194=CARTESIAN_POINT('Origin',(-0.00946837505095689,-0.008,0.00919727535166899));
#34195=CARTESIAN_POINT('',(-0.00963913831581246,-0.008,0.00901468316296458));
#34196=CARTESIAN_POINT('',(-0.00964770033601289,-0.008,0.00937146617272333));
#34197=CARTESIAN_POINT('Origin',(-0.00946837505096689,-0.00799999999999,
0.00919727535167899));
#34198=CARTESIAN_POINT('',(-0.00964770033601289,-0.024,0.00937146617272333));
#34199=CARTESIAN_POINT('',(-0.0096477003360229,-0.00799999999999,0.00937146617273333));
#34200=CARTESIAN_POINT('',(-0.00963913831581246,-0.024,0.00901468316296458));
#34201=CARTESIAN_POINT('Origin',(-0.00946837505096689,-0.02400000000001,
0.00919727535167899));
#34202=CARTESIAN_POINT('',(-0.00963913831582247,-0.00799999999999,0.00901468316297458));
#34203=CARTESIAN_POINT('Origin',(-4.44089209850063E-17,-0.008,6.72997231505748E-33));
#34204=CARTESIAN_POINT('',(-0.00937146617272338,-0.008,0.00964770033601285));
#34205=CARTESIAN_POINT('Origin',(-4.44089209850063E-17,-0.00799999999999,
6.72997231505748E-33));
#34206=CARTESIAN_POINT('',(-0.00937146617272338,-0.024,0.00964770033601285));
#34207=CARTESIAN_POINT('',(-0.00937146617273337,-0.00799999999999,0.00964770033602285));
#34208=CARTESIAN_POINT('Origin',(-4.44089209850063E-17,-0.02400000000001,
6.72997231505748E-33));
#34209=CARTESIAN_POINT('Origin',(-0.00919727535166904,-0.008,0.00946837505095685));
#34210=CARTESIAN_POINT('',(-0.00901468316296463,-0.008,0.00963913831581242));
#34211=CARTESIAN_POINT('Origin',(-0.00919727535167904,-0.00799999999999,
0.00946837505096685));
#34212=CARTESIAN_POINT('',(-0.00901468316296463,-0.024,0.00963913831581242));
#34213=CARTESIAN_POINT('',(-0.00901468316297463,-0.00799999999999,0.00963913831582242));
#34214=CARTESIAN_POINT('Origin',(-0.00919727535167904,-0.02400000000001,
0.00946837505096685));
#34215=CARTESIAN_POINT('Origin',(-0.0088796897724895,-0.008,0.00949479381262943));
#34216=CARTESIAN_POINT('',(-0.0088796897724895,-0.008,0.00949479381262943));
#34217=CARTESIAN_POINT('',(-0.00881874742507032,-0.00799999999999,0.00942962993438206));
#34218=CARTESIAN_POINT('',(-0.0088796897724895,-0.024,0.00949479381262943));
#34219=CARTESIAN_POINT('',(-0.00887968977249951,-0.016,0.00949479381263943));
#34220=CARTESIAN_POINT('',(-0.00881874742507032,-0.02400000000001,0.00942962993438206));
#34221=CARTESIAN_POINT('Origin',(-0.00818688645937852,-0.008,0.010354462327965));
#34222=CARTESIAN_POINT('',(-0.00838002188395169,-0.008,0.0101957213194796));
#34223=CARTESIAN_POINT('',(-0.00834194112716978,-0.008,0.0105505695690249));
#34224=CARTESIAN_POINT('Origin',(-0.00818688645938851,-0.00799999999999,
0.010354462327975));
#34225=CARTESIAN_POINT('',(-0.00834194112716978,-0.024,0.0105505695690249));
#34226=CARTESIAN_POINT('',(-0.00834194112717978,-0.00799999999999,0.0105505695690349));
#34227=CARTESIAN_POINT('',(-0.00838002188395169,-0.024,0.0101957213194796));
#34228=CARTESIAN_POINT('Origin',(-0.00818688645938851,-0.02400000000001,
0.010354462327975));
#34229=CARTESIAN_POINT('',(-0.0083800218839617,-0.00799999999999,0.0101957213194896));
#34230=CARTESIAN_POINT('Origin',(-4.44089209850063E-17,-0.008,6.72997231505748E-33));
#34231=CARTESIAN_POINT('',(-0.00803201439194522,-0.008,0.0107883847172589));
#34232=CARTESIAN_POINT('Origin',(-4.44089209850063E-17,-0.00799999999999,
6.72997231505748E-33));
#34233=CARTESIAN_POINT('',(-0.00803201439194522,-0.024,0.0107883847172589));
#34234=CARTESIAN_POINT('',(-0.00803201439195521,-0.00799999999999,0.0107883847172689));
#34235=CARTESIAN_POINT('Origin',(-4.44089209850063E-17,-0.02400000000001,
6.72997231505748E-33));
#34236=CARTESIAN_POINT('Origin',(-0.00788272044413954,-0.008,0.0105878571202839));
#34237=CARTESIAN_POINT('',(-0.00767940127818889,-0.008,0.0107333264186156));
#34238=CARTESIAN_POINT('Origin',(-0.00788272044414953,-0.00799999999999,
0.0105878571202939));
#34239=CARTESIAN_POINT('',(-0.00767940127818889,-0.024,0.0107333264186156));
#34240=CARTESIAN_POINT('',(-0.00767940127819889,-0.00799999999999,0.0107333264186256));
#34241=CARTESIAN_POINT('Origin',(-0.00788272044414953,-0.02400000000001,
0.0105878571202939));
#34242=CARTESIAN_POINT('Origin',(-0.00756440351325127,-0.008,0.0105725966294337));
#34243=CARTESIAN_POINT('',(-0.00756440351325127,-0.008,0.0105725966294337));
#34244=CARTESIAN_POINT('',(-0.00746427554955181,-0.00799999999999,0.0104326500269426));
#34245=CARTESIAN_POINT('',(-0.00756440351325127,-0.024,0.0105725966294337));
#34246=CARTESIAN_POINT('',(-0.00756440351326127,-0.016,0.0105725966294437));
#34247=CARTESIAN_POINT('',(-0.00746427554955181,-0.02400000000001,0.0104326500269426));
#34248=CARTESIAN_POINT('Origin',(-0.00676531797064642,-0.008,0.0113344815830301));
#34249=CARTESIAN_POINT('',(-0.00697752095427551,-0.008,0.0112023078574304));
#34250=CARTESIAN_POINT('',(-0.00689344899281775,-0.008,0.01154914979483));
#34251=CARTESIAN_POINT('Origin',(-0.00676531797065643,-0.00799999999999,
0.0113344815830401));
#34252=CARTESIAN_POINT('',(-0.00689344899281775,-0.024,0.01154914979483));
#34253=CARTESIAN_POINT('',(-0.00689344899282776,-0.00799999999999,0.0115491497948399));
#34254=CARTESIAN_POINT('',(-0.00697752095427551,-0.024,0.0112023078574304));
#34255=CARTESIAN_POINT('Origin',(-0.00676531797065643,-0.02400000000001,
0.0113344815830401));
#34256=CARTESIAN_POINT('',(-0.00697752095428551,-0.00799999999999,0.0112023078574404));
#34257=CARTESIAN_POINT('Origin',(-4.44089209850063E-17,-0.008,6.72997231505748E-33));
#34258=CARTESIAN_POINT('',(-0.00655513261802576,-0.008,0.0117444768448874));
#34259=CARTESIAN_POINT('Origin',(-4.44089209850063E-17,-0.00799999999999,
6.72997231505748E-33));
#34260=CARTESIAN_POINT('',(-0.00655513261802576,-0.024,0.0117444768448874));
#34261=CARTESIAN_POINT('',(-0.00655513261803576,-0.00799999999999,0.0117444768448974));
#34262=CARTESIAN_POINT('Origin',(-4.44089209850063E-17,-0.02400000000001,
6.72997231505748E-33));
#34263=CARTESIAN_POINT('Origin',(-0.00643329000430782,-0.008,0.0115261780187742));
#34264=CARTESIAN_POINT('',(-0.00621272270841107,-0.008,0.011643864330556));
#34265=CARTESIAN_POINT('Origin',(-0.00643329000431782,-0.00799999999999,
0.0115261780187842));
#34266=CARTESIAN_POINT('',(-0.00621272270841107,-0.024,0.011643864330556));
#34267=CARTESIAN_POINT('',(-0.00621272270842108,-0.00799999999999,0.011643864330566));
#34268=CARTESIAN_POINT('Origin',(-0.00643329000431782,-0.02400000000001,
0.0115261780187842));
#34269=CARTESIAN_POINT('Origin',(-0.00611968821265244,-0.008,0.0114694993866308));
#34270=CARTESIAN_POINT('',(-0.00611968821265244,-0.008,0.0114694993866308));
#34271=CARTESIAN_POINT('',(-0.00594871026243943,-0.00799999999999,0.0111490530784194));
#34272=CARTESIAN_POINT('',(-0.00611968821265244,-0.024,0.0114694993866308));
#34273=CARTESIAN_POINT('',(-0.00611968821266244,-0.016,0.0114694993866408));
#34274=CARTESIAN_POINT('',(-0.00594871026243943,-0.02400000000001,0.0111490530784194));
#34275=CARTESIAN_POINT('Origin',(-0.00711094643726563,-0.008,0.0114165205192449));
#34276=CARTESIAN_POINT('',(-0.00687303373118612,-0.024,0.0110345551487125));
#34277=CARTESIAN_POINT('',(-0.00685869652879269,-0.02400000000001,0.0110115369799216));
#34278=CARTESIAN_POINT('',(-0.00687303373118612,-0.008,0.0110345551487125));
#34279=CARTESIAN_POINT('',(-0.00687303373119612,-0.016,0.0110345551487225));
#34280=CARTESIAN_POINT('',(-0.00685869652879269,-0.00799999999999,0.0110115369799216));
#34281=CARTESIAN_POINT('Origin',(-0.00854026625651055,-0.008,0.010390685842037));
#34282=CARTESIAN_POINT('',(-0.00825453244123696,-0.024,0.0100430420778053));
#34283=CARTESIAN_POINT('',(-0.00832370938221705,-0.02400000000001,0.0101272075873608));
#34284=CARTESIAN_POINT('',(-0.00825453244123696,-0.008,0.0100430420778053));
#34285=CARTESIAN_POINT('',(-0.00825453244124696,-0.016,0.0100430420778153));
#34286=CARTESIAN_POINT('',(-0.00832370938221705,-0.00799999999999,0.0101272075873608));
#34287=CARTESIAN_POINT('Origin',(-0.0109385711281449,-0.008,0.00782624825024839));
#34288=CARTESIAN_POINT('',(-0.0105725966294337,-0.024,0.00756440351325123));
#34289=CARTESIAN_POINT('',(-0.0106156372762982,-0.02400000000001,0.00759519791805035));
#34290=CARTESIAN_POINT('',(-0.0105725966294337,-0.008,0.00756440351325123));
#34291=CARTESIAN_POINT('',(-0.0105725966294437,-0.016,0.00756440351326123));
#34292=CARTESIAN_POINT('',(-0.0106156372762982,-0.00799999999999,0.00759519791805035));
#34293=CARTESIAN_POINT('Origin',(-0.0118665205192449,-0.008,0.0063315235738596));
#34294=CARTESIAN_POINT('',(-0.0114694993866308,-0.024,0.0061196882126524));
#34295=CARTESIAN_POINT('',(-0.0113475636447265,-0.02400000000001,0.00605462794304299));
#34296=CARTESIAN_POINT('',(-0.0114694993866308,-0.008,0.0061196882126524));
#34297=CARTESIAN_POINT('',(-0.0114694993866408,-0.016,0.0061196882126624));
#34298=CARTESIAN_POINT('',(-0.0113475636447265,-0.00799999999999,0.00605462794304299));
#34299=CARTESIAN_POINT('Origin',(-4.44089209850063E-17,-0.016,6.72997231505748E-33));
#34300=CARTESIAN_POINT('',(-0.00559664425850789,-0.008,0.0117336086965482));
#34301=CARTESIAN_POINT('Origin',(-4.44089209850063E-17,-0.00799999999999,
6.72997231505748E-33));
#34302=CARTESIAN_POINT('',(-0.00559664425850789,-0.024,0.0117336086965482));
#34303=CARTESIAN_POINT('',(-0.00559664425851789,-0.016,0.0117336086965582));
#34304=CARTESIAN_POINT('Origin',(-4.44089209850063E-17,-0.02400000000001,
6.72997231505748E-33));
#34305=CARTESIAN_POINT('Origin',(-4.44089209850063E-17,-0.016,6.72997231505748E-33));
#34306=CARTESIAN_POINT('Origin',(-4.44089209850063E-17,-0.02400000000001,
6.72997231505748E-33));
#34307=CARTESIAN_POINT('Origin',(-4.44089209850063E-17,-0.00799999999999,
6.72997231505748E-33));
#34308=CARTESIAN_POINT('Origin',(-0.0090712898554855,-0.024,0.00907128985548545));
#34309=CARTESIAN_POINT('',(-0.00598410424563535,-0.024,0.0125459354524631));
#34310=CARTESIAN_POINT('',(-0.00598410424564535,-0.02400000000001,0.0125459354524731));
#34311=CARTESIAN_POINT('',(-0.0125459354524631,-0.024,0.0059841042456353));
#34312=CARTESIAN_POINT('Origin',(-4.44089209850063E-17,-0.02400000000001,
6.72997231505748E-33));
#34313=CARTESIAN_POINT('',(-0.0117336086965482,-0.024,0.00559664425850784));
#34314=CARTESIAN_POINT('',(-0.0117336086965582,-0.02400000000001,0.00559664425851784));
#34315=CARTESIAN_POINT('Origin',(-4.44089209850063E-17,-0.02400000000001,
6.72997231505748E-33));
#34316=CARTESIAN_POINT('Origin',(-4.44089209850063E-17,-0.02400000000001,
6.72997231505748E-33));
#34317=CARTESIAN_POINT('',(-0.00949479381262948,-0.024,0.00887968977248946));
#34318=CARTESIAN_POINT('Origin',(-4.44089209850063E-17,-0.02400000000001,
6.72997231505748E-33));
#34319=CARTESIAN_POINT('',(-0.00959396290421607,-0.02400000000001,0.00897243436344028));
#34320=CARTESIAN_POINT('Origin',(-4.44089209850063E-17,-0.02400000000001,
6.72997231505748E-33));
#34321=CARTESIAN_POINT('Origin',(-4.44089209850063E-17,-0.016,6.72997231505748E-33));
#34322=CARTESIAN_POINT('',(-0.00949479381262948,-0.008,0.00887968977248946));
#34323=CARTESIAN_POINT('Origin',(-4.44089209850063E-17,-0.00799999999999,
6.72997231505748E-33));
#34324=CARTESIAN_POINT('',(-0.00949479381263948,-0.016,0.00887968977249946));
#34325=CARTESIAN_POINT('Origin',(-4.44089209850063E-17,-0.016,6.72997231505748E-33));
#34326=CARTESIAN_POINT('',(-0.0117336086965482,-0.008,0.00559664425850784));
#34327=CARTESIAN_POINT('',(-0.0117336086965582,-0.016,0.00559664425851784));
#34328=CARTESIAN_POINT('Origin',(-4.44089209850063E-17,-0.00799999999999,
6.72997231505748E-33));
#34329=CARTESIAN_POINT('Origin',(-0.00982345975229741,-0.008,0.00918706364922948));
#34330=CARTESIAN_POINT('',(-0.00959396290421607,-0.00799999999999,0.00897243436344028));
#34331=CARTESIAN_POINT('Origin',(-4.44089209850063E-17,-0.016,6.72997231505748E-33));
#34332=CARTESIAN_POINT('Origin',(-4.44089209850063E-17,-0.00799999999999,
6.72997231505748E-33));
#34333=CARTESIAN_POINT('Origin',(-0.00598410424563535,-0.016,0.0125459354524631));
#34334=CARTESIAN_POINT('',(-0.00598410424563535,-0.008,0.0125459354524631));
#34335=CARTESIAN_POINT('',(-0.00598410424564535,-0.00799999999999,0.0125459354524731));
#34336=CARTESIAN_POINT('',(-0.00598410424564535,-0.016,0.0125459354524731));
#34337=CARTESIAN_POINT('Origin',(-4.44089209850063E-17,-0.016,6.72997231505748E-33));
#34338=CARTESIAN_POINT('',(-0.0125459354524631,-0.008,0.0059841042456353));
#34339=CARTESIAN_POINT('Origin',(-4.44089209850063E-17,-0.00799999999999,
6.72997231505748E-33));
#34340=CARTESIAN_POINT('',(-0.0125459354524731,-0.016,0.0059841042456453));
#34341=CARTESIAN_POINT('Origin',(-0.0117336086965482,-0.016,0.00559664425850784));
#34342=CARTESIAN_POINT('',(-0.0117336086965582,-0.00799999999999,0.00559664425851784));
#34343=CARTESIAN_POINT('Origin',(-4.44089209850063E-17,-0.016,6.72997231505748E-33));
#34344=CARTESIAN_POINT('Origin',(-4.44089209850063E-17,-0.00799999999999,
6.72997231505748E-33));
#34345=CARTESIAN_POINT('Origin',(-0.0090712898554855,-0.008,0.00907128985548545));
#34346=CARTESIAN_POINT('',(0.,0.,0.));
#34347=CARTESIAN_POINT('Origin',(-4.50826289289608E-17,-0.006725,1.13636778952413E-32));
#34348=CARTESIAN_POINT('',(0.00159455284238602,-0.00672500000001,0.00192546130391876));
#34349=CARTESIAN_POINT('',(0.00192546130392509,-0.00672500000001,-0.00159455284237836));
#34350=CARTESIAN_POINT('Origin',(-4.50826289289603E-17,-0.00672500000001,
1.13636778952415E-32));
#34351=CARTESIAN_POINT('',(0.00213726204735601,-0.00700000000001,-0.00176995365503928));
#34352=CARTESIAN_POINT('Origin',(0.00213726204734831,-0.006725,-0.0017699536550329));
#34353=CARTESIAN_POINT('Origin',(-4.50701155292233E-17,-0.00700000000001,
1.13678537952423E-32));
#34354=CARTESIAN_POINT('Origin',(-4.50826289289603E-17,-0.00672500000001,
1.13636778952415E-32));
#34355=CARTESIAN_POINT('Origin',(-4.51838737086513E-17,-0.0045,1.13298910679617E-32));
#34356=CARTESIAN_POINT('',(0.00159455284238602,-0.00227500000001001,0.00192546130391876));
#34357=CARTESIAN_POINT('',(0.00192546130392509,-0.00227500000001001,-0.00159455284237836));
#34358=CARTESIAN_POINT('Origin',(-4.52851184883414E-17,-0.00227500000001001,
1.12961042406822E-32));
#34359=CARTESIAN_POINT('',(0.00159455284237193,-0.0045,0.00192546130391744));
#34360=CARTESIAN_POINT('Origin',(-4.52851184883414E-17,-0.00227500000001001,
1.12961042406822E-32));
#34361=CARTESIAN_POINT('Origin',(-0.00217922221790842,-0.007,-0.0026314637820205));
#34362=CARTESIAN_POINT('',(0.00276389159344472,-0.00700000000001,0.00333746626012356));
#34363=CARTESIAN_POINT('Origin',(-4.50701155292233E-17,-0.00700000000001,
1.13678537952423E-32));
#34364=CARTESIAN_POINT('Origin',(-4.52851184883419E-17,-0.002275,1.1296104240682E-32));
#34365=CARTESIAN_POINT('',(0.00213726204735601,-0.00200000000001001,-0.00176995365503928));
#34366=CARTESIAN_POINT('Origin',(-4.52976318880785E-17,-0.00200000000001001,
1.12919283406813E-32));
#34367=CARTESIAN_POINT('Origin',(0.00213726204734831,-0.002275,-0.0017699536550329));
#34368=CARTESIAN_POINT('Origin',(-0.00217922221790842,-0.002,-0.0026314637820205));
#34369=CARTESIAN_POINT('',(0.00276389159344472,-0.00200000000001001,0.00333746626012356));
#34370=CARTESIAN_POINT('Origin',(-4.52976318880785E-17,-0.00200000000001001,
1.12919283406813E-32));
#34371=CARTESIAN_POINT('Origin',(-4.51838737086513E-17,-0.0045,1.13298910679617E-32));
#34372=CARTESIAN_POINT('',(0.00276389159344472,-0.0045,0.00333746626012356));
#34373=CARTESIAN_POINT('',(0.,0.,0.));
#34374=CARTESIAN_POINT('Origin',(0.02115,-0.0223,-0.01175));
#34375=CARTESIAN_POINT('',(0.02115,-0.02545,-0.00125000000000007));
#34376=CARTESIAN_POINT('',(0.02115,-0.02545,-0.000750000000000074));
#34377=CARTESIAN_POINT('',(0.02115000000001,-0.02545000000001,-0.00649999999999003));
#34378=CARTESIAN_POINT('',(0.02115,-0.0317,-0.000750000000000074));
#34379=CARTESIAN_POINT('',(0.0211500000000101,-0.02545000000001,-0.000749999999990073));
#34380=CARTESIAN_POINT('',(0.02115,-0.0317,-0.00125000000000007));
#34381=CARTESIAN_POINT('',(0.0211500000000101,-0.0317000000000099,-0.00549999999999003));
#34382=CARTESIAN_POINT('',(0.0211500000000101,-0.02545000000001,-0.00124999999999007));
#34383=CARTESIAN_POINT('Origin',(0.02065,-0.02545,-0.000750000000000068));
#34384=CARTESIAN_POINT('',(0.02065,-0.02545,-0.00125000000000007));
#34385=CARTESIAN_POINT('',(0.02065,-0.02545,-0.000750000000000068));
#34386=CARTESIAN_POINT('',(0.0206500000000101,-0.02545000000001,-0.000749999999990068));
#34387=CARTESIAN_POINT('',(0.02065,-0.0317,-0.00125000000000007));
#34388=CARTESIAN_POINT('',(0.0206500000000101,-0.02545000000001,-0.00124999999999007));
#34389=CARTESIAN_POINT('',(0.02065,-0.0317,-0.000750000000000068));
#34390=CARTESIAN_POINT('',(0.0206500000000101,-0.03170000000001,-0.000749999999990068));
#34391=CARTESIAN_POINT('',(0.0206500000000101,-0.02545000000001,-0.000749999999990068));
#34392=CARTESIAN_POINT('Origin',(0.02115,-0.02545,-0.00100000000000007));
#34393=CARTESIAN_POINT('',(0.02115,-0.02495,-0.00125000000000007));
#34394=CARTESIAN_POINT('',(0.02115,-0.02495,-0.000750000000000074));
#34395=CARTESIAN_POINT('',(0.0211500000000101,-0.02495000000001,-0.000749999999990073));
#34396=CARTESIAN_POINT('Origin',(0.0211500000000101,-0.02545000000001,-0.00124999999999007));
#34397=CARTESIAN_POINT('Origin',(0.0211500000000101,-0.02545000000001,-0.000749999999990073));
#34398=CARTESIAN_POINT('Origin',(0.02115,-0.0317,0.000749999999999928));
#34399=CARTESIAN_POINT('',(0.0206500000000101,-0.03170000000001,-0.000749999999990068));
#34400=CARTESIAN_POINT('',(0.0206500000000101,-0.03170000000001,-0.00124999999999007));
#34401=CARTESIAN_POINT('Origin',(0.0229,-0.02495,-0.000750000000000093));
#34402=CARTESIAN_POINT('',(0.0262,-0.02545,-0.000750000000000127));
#34403=CARTESIAN_POINT('',(0.0229000000000101,-0.02545000000001,-0.000749999999990092));
#34404=CARTESIAN_POINT('',(0.0262,-0.02495,-0.000750000000000127));
#34405=CARTESIAN_POINT('',(0.0262000000000101,-0.02545000000001,-0.000749999999990028));
#34406=CARTESIAN_POINT('',(0.0229000000000101,-0.02495000000001,-0.000749999999990092));
#34407=CARTESIAN_POINT('Origin',(0.0229,-0.02495,-0.00125000000000009));
#34408=CARTESIAN_POINT('',(0.0262,-0.02495,-0.00125000000000013));
#34409=CARTESIAN_POINT('',(0.0262000000000101,-0.02495000000001,-0.000749999999990028));
#34410=CARTESIAN_POINT('',(0.0229000000000101,-0.02495000000001,-0.00124999999999009));
#34411=CARTESIAN_POINT('Origin',(0.0229,-0.02545,-0.00125000000000009));
#34412=CARTESIAN_POINT('',(0.0262,-0.02545,-0.00125000000000013));
#34413=CARTESIAN_POINT('',(0.0262000000000102,-0.02495000000001,-0.00124999999999003));
#34414=CARTESIAN_POINT('',(0.0229000000000101,-0.02545000000001,-0.00124999999999009));
#34415=CARTESIAN_POINT('Origin',(0.0229,-0.02545,-0.000750000000000093));
#34416=CARTESIAN_POINT('',(0.0262000000000102,-0.02545000000001,-0.00124999999999003));
#34417=CARTESIAN_POINT('Origin',(0.0262,-0.0252,-0.00100000000000013));
#34418=CARTESIAN_POINT('',(0.,0.,0.));
#34419=CARTESIAN_POINT('Origin',(0.0155,-0.0056534125,0.0155));
#34420=CARTESIAN_POINT('',(0.01700000000002,-0.00580682499999,0.0155));
#34421=CARTESIAN_POINT('',(0.013999999999995,-0.005806825000005,0.0155));
#34422=CARTESIAN_POINT('Origin',(0.01550000000001,-0.00580682499999,0.0155));
#34423=CARTESIAN_POINT('',(0.01430672500001,-0.00549999999998999,0.0155));
#34424=CARTESIAN_POINT('',(0.0141533625,-0.0056534125,0.0155));
#34425=CARTESIAN_POINT('Origin',(0.01550000000001,-0.00549999999999,0.0155));
#34426=CARTESIAN_POINT('Origin',(0.01550000000001,-0.00580682499999,0.0155));
#34427=CARTESIAN_POINT('Origin',(0.0155,-0.0175,0.0155));
#34428=CARTESIAN_POINT('',(0.017,-0.02949999999999,0.0155));
#34429=CARTESIAN_POINT('',(0.017,-0.0175,0.0155));
#34430=CARTESIAN_POINT('Origin',(0.01550000000001,-0.02949999999999,0.0155));
#34431=CARTESIAN_POINT('Origin',(0.01475,-0.0055,0.0155));
#34432=CARTESIAN_POINT('Origin',(0.0155,-0.0325967679907942,0.0155));
#34433=CARTESIAN_POINT('',(0.0140430296811173,-0.0326789662095993,0.0153032273967176));
#34434=CARTESIAN_POINT('',(0.0141463367962054,-0.0326351410015245,0.0153028384738583));
#34435=CARTESIAN_POINT('Ctrl Pts',(0.0141463367962063,-0.0326351410015253,
0.015302838473864));
#34436=CARTESIAN_POINT('Ctrl Pts',(0.0141423240437266,-0.032643263445668,
0.0153022914211073));
#34437=CARTESIAN_POINT('Ctrl Pts',(0.0141364374786249,-0.032651336899898,
0.0153018253164866));
#34438=CARTESIAN_POINT('Ctrl Pts',(0.0141228216222177,-0.0326649719690126,
0.0153011884352657));
#34439=CARTESIAN_POINT('Ctrl Pts',(0.0141121610166096,-0.032672062422094,
0.0153010037121127));
#34440=CARTESIAN_POINT('Ctrl Pts',(0.0140922949035023,-0.0326802644698773,
0.0153010982569886));
#34441=CARTESIAN_POINT('Ctrl Pts',(0.0140795551609431,-0.0326827679907942,
0.0153014002324808));
#34442=CARTESIAN_POINT('Ctrl Pts',(0.0140605993929865,-0.0326827679907942,
0.0153021757211875));
#34443=CARTESIAN_POINT('Ctrl Pts',(0.0140513381771173,-0.0326814761879823,
0.0153026677141935));
#34444=CARTESIAN_POINT('Ctrl Pts',(0.0140430296811173,-0.0326789662095993,
0.0153032273967175));
#34445=CARTESIAN_POINT('',(0.0141463367962067,-0.0326351410015237,0.0156971615261415));
#34446=CARTESIAN_POINT('Origin',(0.0155,-0.0326351410027316,0.01549999999999));
#34447=CARTESIAN_POINT('',(0.0140430296811173,-0.0326789662095993,0.0156967726032824));
#34448=CARTESIAN_POINT('Ctrl Pts',(0.0140430296811173,-0.0326789662095993,
0.0156967726032824));
#34449=CARTESIAN_POINT('Ctrl Pts',(0.0140513381771173,-0.0326814761879823,
0.0156973322858065));
#34450=CARTESIAN_POINT('Ctrl Pts',(0.0140605993929865,-0.0326827679907942,
0.0156978242788125));
#34451=CARTESIAN_POINT('Ctrl Pts',(0.0140795551609431,-0.0326827679907942,
0.0156985997675192));
#34452=CARTESIAN_POINT('Ctrl Pts',(0.0140922949035023,-0.0326802644698773,
0.0156989017430114));
#34453=CARTESIAN_POINT('Ctrl Pts',(0.0141121610166096,-0.032672062422094,
0.0156989962878872));
#34454=CARTESIAN_POINT('Ctrl Pts',(0.0141228216222177,-0.0326649719690126,
0.0156988115647342));
#34455=CARTESIAN_POINT('Ctrl Pts',(0.0141364374786252,-0.0326513368998977,
0.0156981746835134));
#34456=CARTESIAN_POINT('Ctrl Pts',(0.0141423240437271,-0.0326432634456672,
0.0156977085788927));
#34457=CARTESIAN_POINT('Ctrl Pts',(0.0141463367962069,-0.0326351410015241,
0.0156971615261359));
#34458=CARTESIAN_POINT('Origin',(0.01549999999999,-0.0326789662096093,0.0155));
#34459=CARTESIAN_POINT('Origin',(0.0155,-0.0321179414315921,0.0155));
#34460=CARTESIAN_POINT('',(0.0146893860964955,-0.0315359551043615,0.0153768688374301));
#34461=CARTESIAN_POINT('Ctrl Pts',(0.0141463367962063,-0.0326351410015253,
0.015302838473864));
#34462=CARTESIAN_POINT('Ctrl Pts',(0.0144860139927036,-0.0319475807897096,
0.0153491461736378));
#34463=CARTESIAN_POINT('Ctrl Pts',(0.0146893860964955,-0.0315359551043615,
0.0153768688374301));
#34464=CARTESIAN_POINT('',(0.0146893860964955,-0.0315359551043615,0.0156231311625699));
#34465=CARTESIAN_POINT('Origin',(0.01550000000001,-0.0315359551043715,0.0155));
#34466=CARTESIAN_POINT('Ctrl Pts',(0.0146893860964954,-0.0315359551043615,
0.0156231311625699));
#34467=CARTESIAN_POINT('Ctrl Pts',(0.0144860139924889,-0.0319475807901437,
0.0156508538263914));
#34468=CARTESIAN_POINT('Ctrl Pts',(0.0141463367962068,-0.0326351410015241,
0.0156971615261359));
#34469=CARTESIAN_POINT('Origin',(0.0155,-0.0325967679907942,0.0155));
#34470=CARTESIAN_POINT('',(0.0156967726032824,-0.0326789662095993,0.0140430296811173));
#34471=CARTESIAN_POINT('',(0.0156971615261417,-0.0326351410015244,0.0141463367962054));
#34472=CARTESIAN_POINT('Ctrl Pts',(0.015697161526136,-0.0326351410015253,
0.0141463367962063));
#34473=CARTESIAN_POINT('Ctrl Pts',(0.0156977085788927,-0.032643263445668,
0.0141423240437266));
#34474=CARTESIAN_POINT('Ctrl Pts',(0.0156981746835134,-0.032651336899898,
0.0141364374786249));
#34475=CARTESIAN_POINT('Ctrl Pts',(0.0156988115647343,-0.0326649719690126,
0.0141228216222177));
#34476=CARTESIAN_POINT('Ctrl Pts',(0.0156989962878873,-0.032672062422094,
0.0141121610166096));
#34477=CARTESIAN_POINT('Ctrl Pts',(0.0156989017430114,-0.0326802644698773,
0.0140922949035023));
#34478=CARTESIAN_POINT('Ctrl Pts',(0.0156985997675192,-0.0326827679907942,
0.0140795551609431));
#34479=CARTESIAN_POINT('Ctrl Pts',(0.0156978242788125,-0.0326827679907942,
0.0140605993929865));
#34480=CARTESIAN_POINT('Ctrl Pts',(0.0156973322858065,-0.0326814761879823,
0.0140513381771173));
#34481=CARTESIAN_POINT('Ctrl Pts',(0.0156967726032825,-0.0326789662095993,
0.0140430296811173));
#34482=CARTESIAN_POINT('',(0.0153028384738585,-0.0326351410015237,0.0141463367962067));
#34483=CARTESIAN_POINT('Origin',(0.01550000000001,-0.0326351410027316,0.0155));
#34484=CARTESIAN_POINT('',(0.0153032273967176,-0.0326789662095993,0.0140430296811173));
#34485=CARTESIAN_POINT('Ctrl Pts',(0.0153032273967176,-0.0326789662095993,
0.0140430296811173));
#34486=CARTESIAN_POINT('Ctrl Pts',(0.0153026677141935,-0.0326814761879823,
0.0140513381771173));
#34487=CARTESIAN_POINT('Ctrl Pts',(0.0153021757211875,-0.0326827679907942,
0.0140605993929865));
#34488=CARTESIAN_POINT('Ctrl Pts',(0.0153014002324808,-0.0326827679907942,
0.0140795551609431));
#34489=CARTESIAN_POINT('Ctrl Pts',(0.0153010982569886,-0.0326802644698773,
0.0140922949035023));
#34490=CARTESIAN_POINT('Ctrl Pts',(0.0153010037121128,-0.032672062422094,
0.0141121610166096));
#34491=CARTESIAN_POINT('Ctrl Pts',(0.0153011884352658,-0.0326649719690126,
0.0141228216222177));
#34492=CARTESIAN_POINT('Ctrl Pts',(0.0153018253164866,-0.0326513368998977,
0.0141364374786252));
#34493=CARTESIAN_POINT('Ctrl Pts',(0.0153022914211073,-0.0326432634456672,
0.0141423240437272));
#34494=CARTESIAN_POINT('Ctrl Pts',(0.0153028384738641,-0.0326351410015241,
0.0141463367962069));
#34495=CARTESIAN_POINT('Origin',(0.01549999999999,-0.0326789662096093,0.0155));
#34496=CARTESIAN_POINT('Origin',(0.0155,-0.0321179414315921,0.0155));
#34497=CARTESIAN_POINT('',(0.0156231311625699,-0.0315359551043615,0.0146893860964955));
#34498=CARTESIAN_POINT('Ctrl Pts',(0.015697161526136,-0.0326351410015253,
0.0141463367962062));
#34499=CARTESIAN_POINT('Ctrl Pts',(0.0156508538263853,-0.0319475807900528,
0.0144860139925339));
#34500=CARTESIAN_POINT('Ctrl Pts',(0.0156231311625699,-0.0315359551043615,
0.0146893860964954));
#34501=CARTESIAN_POINT('',(0.0153768688374301,-0.0315359551043615,0.0146893860964955));
#34502=CARTESIAN_POINT('Origin',(0.01550000000001,-0.0315359551043715,0.0155));
#34503=CARTESIAN_POINT('Ctrl Pts',(0.0153768688374302,-0.0315359551043615,
0.0146893860964954));
#34504=CARTESIAN_POINT('Ctrl Pts',(0.015349146173611,-0.0319475807901076,
0.0144860139925067));
#34505=CARTESIAN_POINT('Ctrl Pts',(0.0153028384738641,-0.0326351410015241,
0.0141463367962068));
#34506=CARTESIAN_POINT('Origin',(0.0155,-0.0325967679907942,0.0155));
#34507=CARTESIAN_POINT('',(0.0169569703188827,-0.0326789662095993,0.0156967726032824));
#34508=CARTESIAN_POINT('',(0.0168536632037933,-0.0326351410015237,0.0156971615261415));
#34509=CARTESIAN_POINT('Ctrl Pts',(0.0168536632037931,-0.0326351410015241,
0.0156971615261359));
#34510=CARTESIAN_POINT('Ctrl Pts',(0.0168576759562728,-0.0326432634456672,
0.0156977085788927));
#34511=CARTESIAN_POINT('Ctrl Pts',(0.0168635625213748,-0.0326513368998977,
0.0156981746835134));
#34512=CARTESIAN_POINT('Ctrl Pts',(0.0168771783777823,-0.0326649719690126,
0.0156988115647343));
#34513=CARTESIAN_POINT('Ctrl Pts',(0.0168878389833904,-0.032672062422094,
0.0156989962878873));
#34514=CARTESIAN_POINT('Ctrl Pts',(0.0169077050964977,-0.0326802644698773,
0.0156989017430114));
#34515=CARTESIAN_POINT('Ctrl Pts',(0.0169204448390569,-0.0326827679907942,
0.0156985997675192));
#34516=CARTESIAN_POINT('Ctrl Pts',(0.0169394006070135,-0.0326827679907942,
0.0156978242788125));
#34517=CARTESIAN_POINT('Ctrl Pts',(0.0169486618228827,-0.0326814761879823,
0.0156973322858065));
#34518=CARTESIAN_POINT('Ctrl Pts',(0.0169569703188827,-0.0326789662095993,
0.0156967726032825));
#34519=CARTESIAN_POINT('',(0.0168536632037947,-0.0326351410015244,0.0153028384738584));
#34520=CARTESIAN_POINT('Origin',(0.0155,-0.0326351410027316,0.01549999999999));
#34521=CARTESIAN_POINT('',(0.0169569703188827,-0.0326789662095993,0.0153032273967176));
#34522=CARTESIAN_POINT('Ctrl Pts',(0.0169569703188827,-0.0326789662095993,
0.0153032273967176));
#34523=CARTESIAN_POINT('Ctrl Pts',(0.0169486618228827,-0.0326814761879823,
0.0153026677141935));
#34524=CARTESIAN_POINT('Ctrl Pts',(0.0169394006070135,-0.0326827679907942,
0.0153021757211875));
#34525=CARTESIAN_POINT('Ctrl Pts',(0.0169204448390569,-0.0326827679907942,
0.0153014002324808));
#34526=CARTESIAN_POINT('Ctrl Pts',(0.0169077050964977,-0.0326802644698773,
0.0153010982569886));
#34527=CARTESIAN_POINT('Ctrl Pts',(0.0168878389833904,-0.032672062422094,
0.0153010037121128));
#34528=CARTESIAN_POINT('Ctrl Pts',(0.0168771783777823,-0.0326649719690126,
0.0153011884352658));
#34529=CARTESIAN_POINT('Ctrl Pts',(0.0168635625213751,-0.032651336899898,
0.0153018253164866));
#34530=CARTESIAN_POINT('Ctrl Pts',(0.0168576759562734,-0.032643263445668,
0.0153022914211073));
#34531=CARTESIAN_POINT('Ctrl Pts',(0.0168536632037937,-0.0326351410015253,
0.015302838473864));
#34532=CARTESIAN_POINT('Origin',(0.01549999999999,-0.0326789662096093,0.0155));
#34533=CARTESIAN_POINT('Origin',(0.0155,-0.0321179414315921,0.0155));
#34534=CARTESIAN_POINT('',(0.0163106139035045,-0.0315359551043615,0.0156231311625699));
#34535=CARTESIAN_POINT('Ctrl Pts',(0.0168536632037932,-0.0326351410015241,
0.0156971615261359));
#34536=CARTESIAN_POINT('Ctrl Pts',(0.0165139860074969,-0.0319475807901151,
0.0156508538263895));
#34537=CARTESIAN_POINT('Ctrl Pts',(0.0163106139035046,-0.0315359551043615,
0.0156231311625699));
#34538=CARTESIAN_POINT('',(0.0163199123024952,-0.0315359551043719,0.0155));
#34539=CARTESIAN_POINT('Origin',(0.01550000000001,-0.0315359551043715,0.0155));
#34540=CARTESIAN_POINT('',(0.0163106139035045,-0.0315359551043615,0.0153768688374301));
#34541=CARTESIAN_POINT('Origin',(0.01550000000001,-0.0315359551043715,0.0155));
#34542=CARTESIAN_POINT('Ctrl Pts',(0.0163106139035046,-0.0315359551043614,
0.0153768688374302));
#34543=CARTESIAN_POINT('Ctrl Pts',(0.0165139860075985,-0.0319475807903205,
0.0153491461735967));
#34544=CARTESIAN_POINT('Ctrl Pts',(0.0168536632037939,-0.0326351410015252,
0.0153028384738641));
#34545=CARTESIAN_POINT('Origin',(0.0155,-0.0325967679907942,0.0155));
#34546=CARTESIAN_POINT('',(0.0153032273967176,-0.0326789662095993,0.0169569703188827));
#34547=CARTESIAN_POINT('',(0.0153028384738585,-0.0326351410015237,0.0168536632037933));
#34548=CARTESIAN_POINT('Ctrl Pts',(0.0153028384738641,-0.0326351410015241,
0.0168536632037931));
#34549=CARTESIAN_POINT('Ctrl Pts',(0.0153022914211073,-0.0326432634456672,
0.0168576759562728));
#34550=CARTESIAN_POINT('Ctrl Pts',(0.0153018253164866,-0.0326513368998977,
0.0168635625213748));
#34551=CARTESIAN_POINT('Ctrl Pts',(0.0153011884352657,-0.0326649719690126,
0.0168771783777823));
#34552=CARTESIAN_POINT('Ctrl Pts',(0.0153010037121127,-0.032672062422094,
0.0168878389833904));
#34553=CARTESIAN_POINT('Ctrl Pts',(0.0153010982569886,-0.0326802644698773,
0.0169077050964977));
#34554=CARTESIAN_POINT('Ctrl Pts',(0.0153014002324808,-0.0326827679907942,
0.0169204448390569));
#34555=CARTESIAN_POINT('Ctrl Pts',(0.0153021757211875,-0.0326827679907942,
0.0169394006070135));
#34556=CARTESIAN_POINT('Ctrl Pts',(0.0153026677141935,-0.0326814761879823,
0.0169486618228827));
#34557=CARTESIAN_POINT('Ctrl Pts',(0.0153032273967175,-0.0326789662095993,
0.0169569703188827));
#34558=CARTESIAN_POINT('',(0.0156971615261417,-0.0326351410015245,0.0168536632037946));
#34559=CARTESIAN_POINT('Origin',(0.01550000000001,-0.0326351410027316,0.0155));
#34560=CARTESIAN_POINT('',(0.0156967726032824,-0.0326789662095993,0.0169569703188827));
#34561=CARTESIAN_POINT('Ctrl Pts',(0.0156967726032824,-0.0326789662095993,
0.0169569703188827));
#34562=CARTESIAN_POINT('Ctrl Pts',(0.0156973322858065,-0.0326814761879823,
0.0169486618228827));
#34563=CARTESIAN_POINT('Ctrl Pts',(0.0156978242788125,-0.0326827679907942,
0.0169394006070135));
#34564=CARTESIAN_POINT('Ctrl Pts',(0.0156985997675192,-0.0326827679907942,
0.0169204448390569));
#34565=CARTESIAN_POINT('Ctrl Pts',(0.0156989017430114,-0.0326802644698773,
0.0169077050964977));
#34566=CARTESIAN_POINT('Ctrl Pts',(0.0156989962878872,-0.032672062422094,
0.0168878389833904));
#34567=CARTESIAN_POINT('Ctrl Pts',(0.0156988115647342,-0.0326649719690126,
0.0168771783777823));
#34568=CARTESIAN_POINT('Ctrl Pts',(0.0156981746835134,-0.032651336899898,
0.0168635625213751));
#34569=CARTESIAN_POINT('Ctrl Pts',(0.0156977085788927,-0.032643263445668,
0.0168576759562734));
#34570=CARTESIAN_POINT('Ctrl Pts',(0.015697161526136,-0.0326351410015253,
0.0168536632037937));
#34571=CARTESIAN_POINT('Origin',(0.01549999999999,-0.0326789662096093,0.0155));
#34572=CARTESIAN_POINT('Origin',(0.0155,-0.0321179414315921,0.0155));
#34573=CARTESIAN_POINT('',(0.0153768688374301,-0.0315359551043615,0.0163106139035045));
#34574=CARTESIAN_POINT('Ctrl Pts',(0.0153028384738641,-0.0326351410015241,
0.0168536632037932));
#34575=CARTESIAN_POINT('Ctrl Pts',(0.0153491461736176,-0.0319475807900087,
0.0165139860074444));
#34576=CARTESIAN_POINT('Ctrl Pts',(0.0153768688374301,-0.0315359551043615,
0.0163106139035046));
#34577=CARTESIAN_POINT('',(0.0156231311625699,-0.0315359551043615,0.0163106139035045));
#34578=CARTESIAN_POINT('Origin',(0.01550000000001,-0.0315359551043715,0.0155));
#34579=CARTESIAN_POINT('Ctrl Pts',(0.0156231311625699,-0.0315359551043615,
0.0163106139035045));
#34580=CARTESIAN_POINT('Ctrl Pts',(0.0156508538263448,-0.0319475807894513,
0.0165139860071687));
#34581=CARTESIAN_POINT('Ctrl Pts',(0.015697161526136,-0.0326351410015254,
0.0168536632037936));
#34582=CARTESIAN_POINT('Origin',(0.0155,-0.0314896193890613,0.0155));
#34583=CARTESIAN_POINT('',(0.0182642230121603,-0.0315245188857739,0.01549999999999));
#34584=CARTESIAN_POINT('',(0.0155,-0.0315245188857739,0.0182642230121503));
#34585=CARTESIAN_POINT('Origin',(0.0155,-0.0315245188857739,0.01549999999999));
#34586=CARTESIAN_POINT('',(0.0155,-0.0323870242363267,0.017706040231424));
#34587=CARTESIAN_POINT('Origin',(0.0155,-0.0314896193890613,0.0172648321851312));
#34588=CARTESIAN_POINT('Origin',(0.01550000000001,-0.0323870242363367,0.0155));
#34589=CARTESIAN_POINT('Origin',(0.0155,-0.0315245188857739,0.01549999999999));
#34590=CARTESIAN_POINT('Origin',(0.0155,-0.0279,0.0155));
#34591=CARTESIAN_POINT('',(0.0150423056295014,-0.0328724938596638,0.0157545990550246));
#34592=CARTESIAN_POINT('Origin',(0.0155065692871957,-0.0279140604449322,
0.0153394226989194));
#34593=CARTESIAN_POINT('',(0.0152454009449754,-0.0328724938596638,0.0159576943704986));
#34594=CARTESIAN_POINT('Ctrl Pts',(0.0150423056295014,-0.0328724938596638,
0.0157545990550246));
#34595=CARTESIAN_POINT('Ctrl Pts',(0.0150636146923879,-0.0328744020667681,
0.0157556379041868));
#34596=CARTESIAN_POINT('Ctrl Pts',(0.0150856203042815,-0.0328760596977499,
0.0157600236941645));
#34597=CARTESIAN_POINT('Ctrl Pts',(0.0151328421380346,-0.0328788497729191,
0.0157775788158223));
#34598=CARTESIAN_POINT('Ctrl Pts',(0.0151572787782427,-0.0328797021837751,
0.0157929445962307));
#34599=CARTESIAN_POINT('Ctrl Pts',(0.0151963759161913,-0.0328799869200382,
0.0158290125584882));
#34600=CARTESIAN_POINT('Ctrl Pts',(0.0152136491665739,-0.032879439770222,
0.0158521091581119));
#34601=CARTESIAN_POINT('Ctrl Pts',(0.0152375167802226,-0.0328768773126286,
0.0159032280479782));
#34602=CARTESIAN_POINT('Ctrl Pts',(0.0152441117443853,-0.0328748619240703,
0.0159312500536082));
#34603=CARTESIAN_POINT('Ctrl Pts',(0.0152454009449754,-0.0328724938596638,
0.0159576943704985));
#34604=CARTESIAN_POINT('Origin',(0.0156605773010806,-0.0279140604449322,
0.0154934307128043));
#34605=CARTESIAN_POINT('',(0.0157545990550246,-0.0328724938596638,0.0159576943704986));
#34606=CARTESIAN_POINT('Origin',(0.0153394226989194,-0.0279140604449322,
0.0154934307128043));
#34607=CARTESIAN_POINT('',(0.0159576943704986,-0.0328724938596638,0.0157545990550246));
#34608=CARTESIAN_POINT('Ctrl Pts',(0.0157545990550246,-0.0328724938596638,
0.0159576943704986));
#34609=CARTESIAN_POINT('Ctrl Pts',(0.0157556379041868,-0.0328744020667681,
0.0159363853076121));
#34610=CARTESIAN_POINT('Ctrl Pts',(0.0157600236941645,-0.0328760596977499,
0.0159143796957185));
#34611=CARTESIAN_POINT('Ctrl Pts',(0.0157775788158223,-0.0328788497729191,
0.0158671578619654));
#34612=CARTESIAN_POINT('Ctrl Pts',(0.0157929445962307,-0.0328797021837751,
0.0158427212217573));
#34613=CARTESIAN_POINT('Ctrl Pts',(0.0158290125584882,-0.0328799869200382,
0.0158036240838087));
#34614=CARTESIAN_POINT('Ctrl Pts',(0.0158521091581119,-0.032879439770222,
0.0157863508334262));
#34615=CARTESIAN_POINT('Ctrl Pts',(0.0159032280479782,-0.0328768773126286,
0.0157624832197774));
#34616=CARTESIAN_POINT('Ctrl Pts',(0.0159312500536082,-0.0328748619240703,
0.0157558882556147));
#34617=CARTESIAN_POINT('Ctrl Pts',(0.0159576943704985,-0.0328724938596638,
0.0157545990550246));
#34618=CARTESIAN_POINT('Origin',(0.0154934307128043,-0.0279140604449322,
0.0153394226989194));
#34619=CARTESIAN_POINT('',(0.0159576943704986,-0.0328724938596638,0.0152454009449754));
#34620=CARTESIAN_POINT('Origin',(0.0154934307128043,-0.0279140604449322,
0.0156605773010806));
#34621=CARTESIAN_POINT('',(0.0157545990550246,-0.0328724938596638,0.0150423056295014));
#34622=CARTESIAN_POINT('Ctrl Pts',(0.0159576943704986,-0.0328724938596638,
0.0152454009449754));
#34623=CARTESIAN_POINT('Ctrl Pts',(0.0159363853076121,-0.0328744020667681,
0.0152443620958132));
#34624=CARTESIAN_POINT('Ctrl Pts',(0.0159143796957185,-0.0328760596977499,
0.0152399763058355));
#34625=CARTESIAN_POINT('Ctrl Pts',(0.0158671578619654,-0.0328788497729191,
0.0152224211841777));
#34626=CARTESIAN_POINT('Ctrl Pts',(0.0158427212217573,-0.0328797021837751,
0.0152070554037693));
#34627=CARTESIAN_POINT('Ctrl Pts',(0.0158036240838087,-0.0328799869200382,
0.0151709874415118));
#34628=CARTESIAN_POINT('Ctrl Pts',(0.0157863508334262,-0.032879439770222,
0.0151478908418881));
#34629=CARTESIAN_POINT('Ctrl Pts',(0.0157624832197774,-0.0328768773126286,
0.0150967719520218));
#34630=CARTESIAN_POINT('Ctrl Pts',(0.0157558882556147,-0.0328748619240703,
0.0150687499463918));
#34631=CARTESIAN_POINT('Ctrl Pts',(0.0157545990550246,-0.0328724938596638,
0.0150423056295015));
#34632=CARTESIAN_POINT('Origin',(0.0153394226989194,-0.0279140604449322,
0.0155065692871957));
#34633=CARTESIAN_POINT('',(0.0152454009449754,-0.0328724938596638,0.0150423056295014));
#34634=CARTESIAN_POINT('Origin',(0.0156605773010806,-0.0279140604449322,
0.0155065692871957));
#34635=CARTESIAN_POINT('',(0.0150423056295014,-0.0328724938596638,0.0152454009449754));
#34636=CARTESIAN_POINT('Ctrl Pts',(0.0152454009449754,-0.0328724938596638,
0.0150423056295014));
#34637=CARTESIAN_POINT('Ctrl Pts',(0.0152443620958132,-0.0328744020667681,
0.0150636146923879));
#34638=CARTESIAN_POINT('Ctrl Pts',(0.0152399763058355,-0.0328760596977499,
0.0150856203042815));
#34639=CARTESIAN_POINT('Ctrl Pts',(0.0152224211841777,-0.0328788497729191,
0.0151328421380346));
#34640=CARTESIAN_POINT('Ctrl Pts',(0.0152070554037693,-0.0328797021837751,
0.0151572787782427));
#34641=CARTESIAN_POINT('Ctrl Pts',(0.0151709874415118,-0.0328799869200382,
0.0151963759161913));
#34642=CARTESIAN_POINT('Ctrl Pts',(0.0151478908418881,-0.032879439770222,
0.0152136491665738));
#34643=CARTESIAN_POINT('Ctrl Pts',(0.0150967719520218,-0.0328768773126286,
0.0152375167802226));
#34644=CARTESIAN_POINT('Ctrl Pts',(0.0150687499463918,-0.0328748619240703,
0.0152441117443853));
#34645=CARTESIAN_POINT('Ctrl Pts',(0.0150423056295015,-0.0328724938596638,
0.0152454009449754));
#34646=CARTESIAN_POINT('Origin',(0.0155065692871957,-0.0279140604449322,
0.0156605773010806));
#34647=CARTESIAN_POINT('Origin',(0.0155,-0.0312896042064176,0.0155));
#34648=CARTESIAN_POINT('',(0.0183,-0.0304999999999993,0.0155));
#34649=CARTESIAN_POINT('Origin',(0.01550000000001,-0.0305,0.0155));
#34650=CARTESIAN_POINT('',(0.018272426413518,-0.0312896042064176,0.0155));
#34651=CARTESIAN_POINT('Origin',(0.0150336424994489,-0.0329,0.0159663575005511));
#34652=CARTESIAN_POINT('',(0.0150477540341485,-0.0313489793100506,0.0156214202049252));
#34653=CARTESIAN_POINT('',(0.0150422072618173,-0.03290000000001,0.0157570035192005));
#34654=CARTESIAN_POINT('',(0.0153785797950748,-0.0313489793100506,0.0159522459658515));
#34655=CARTESIAN_POINT('Ctrl Pts',(0.0150477540341485,-0.0313489793100505,
0.0156214202049251));
#34656=CARTESIAN_POINT('Ctrl Pts',(0.015081225181466,-0.031331772155721,
0.0156212828339097));
#34657=CARTESIAN_POINT('Ctrl Pts',(0.0151152486469788,-0.0313150763778198,
0.0156263588605475));
#34658=CARTESIAN_POINT('Ctrl Pts',(0.0151692545989321,-0.0312913221771079,
0.015642486377087));
#34659=CARTESIAN_POINT('Ctrl Pts',(0.0151943811304251,-0.0312812420230617,
0.015652929486056));
#34660=CARTESIAN_POINT('Ctrl Pts',(0.0152419157873653,-0.0312670678991654,
0.015680782378196));
#34661=CARTESIAN_POINT('Ctrl Pts',(0.0152643516916966,-0.031263124157519,
0.0156982209860465));
#34662=CARTESIAN_POINT('Ctrl Pts',(0.0153017790139535,-0.031263124157519,
0.0157356483083034));
#34663=CARTESIAN_POINT('Ctrl Pts',(0.015319217621804,-0.0312670678991654,
0.0157580842126347));
#34664=CARTESIAN_POINT('Ctrl Pts',(0.015347070513944,-0.0312812420230617,
0.0158056188695749));
#34665=CARTESIAN_POINT('Ctrl Pts',(0.015357513622913,-0.0312913221771079,
0.0158307454010679));
#34666=CARTESIAN_POINT('Ctrl Pts',(0.0153736411394525,-0.0313150763778198,
0.0158847513530212));
#34667=CARTESIAN_POINT('Ctrl Pts',(0.0153787171660903,-0.031331772155721,
0.015918774818534));
#34668=CARTESIAN_POINT('Ctrl Pts',(0.0153785797950749,-0.0313489793100505,
0.0159522459658515));
#34669=CARTESIAN_POINT('',(0.0152429964807995,-0.03290000000001,0.0159577927381827));
#34670=CARTESIAN_POINT('Origin',(0.0140154882957686,-0.0329,0.015715));
#34671=CARTESIAN_POINT('Ctrl Pts',(0.0150477540341385,-0.0313489793100606,
0.0156214202049351));
#34672=CARTESIAN_POINT('Ctrl Pts',(0.0149179093434978,-0.031415731059247,
0.0156219531085977));
#34673=CARTESIAN_POINT('Ctrl Pts',(0.0146893860964855,-0.0315359551043715,
0.0156231311625798));
#34674=CARTESIAN_POINT('Origin',(0.0150422072618273,-0.0329,0.0152429964808095));
#34675=CARTESIAN_POINT('',(0.0150477540341485,-0.0313489793100506,0.0153785797950748));
#34676=CARTESIAN_POINT('',(0.0150422072618173,-0.03290000000001,0.0152429964807995));
#34677=CARTESIAN_POINT('Ctrl Pts',(0.0146893860964855,-0.0315359551043715,
0.0153768688374201));
#34678=CARTESIAN_POINT('Ctrl Pts',(0.0149179093434978,-0.031415731059247,
0.0153780468914023));
#34679=CARTESIAN_POINT('Ctrl Pts',(0.0150477540341385,-0.0313489793100605,
0.0153785797950649));
#34680=CARTESIAN_POINT('Origin',(0.0150336424994489,-0.0329,0.0150336424994489));
#34681=CARTESIAN_POINT('',(0.0153785797950748,-0.0313489793100506,0.0150477540341485));
#34682=CARTESIAN_POINT('',(0.0152429964807995,-0.03290000000001,0.0150422072618173));
#34683=CARTESIAN_POINT('Ctrl Pts',(0.0153785797950749,-0.0313489793100505,
0.0150477540341485));
#34684=CARTESIAN_POINT('Ctrl Pts',(0.0153787171660903,-0.031331772155721,
0.015081225181466));
#34685=CARTESIAN_POINT('Ctrl Pts',(0.0153736411394525,-0.0313150763778198,
0.0151152486469788));
#34686=CARTESIAN_POINT('Ctrl Pts',(0.015357513622913,-0.0312913221771079,
0.0151692545989321));
#34687=CARTESIAN_POINT('Ctrl Pts',(0.015347070513944,-0.0312812420230617,
0.0151943811304251));
#34688=CARTESIAN_POINT('Ctrl Pts',(0.015319217621804,-0.0312670678991654,
0.0152419157873653));
#34689=CARTESIAN_POINT('Ctrl Pts',(0.0153017790139535,-0.031263124157519,
0.0152643516916966));
#34690=CARTESIAN_POINT('Ctrl Pts',(0.0152643516916966,-0.031263124157519,
0.0153017790139535));
#34691=CARTESIAN_POINT('Ctrl Pts',(0.0152419157873653,-0.0312670678991654,
0.015319217621804));
#34692=CARTESIAN_POINT('Ctrl Pts',(0.0151943811304251,-0.0312812420230617,
0.015347070513944));
#34693=CARTESIAN_POINT('Ctrl Pts',(0.0151692545989321,-0.0312913221771079,
0.015357513622913));
#34694=CARTESIAN_POINT('Ctrl Pts',(0.0151152486469788,-0.0313150763778198,
0.0153736411394525));
#34695=CARTESIAN_POINT('Ctrl Pts',(0.015081225181466,-0.031331772155721,
0.0153787171660903));
#34696=CARTESIAN_POINT('Ctrl Pts',(0.0150477540341485,-0.0313489793100505,
0.0153785797950749));
#34697=CARTESIAN_POINT('Origin',(0.0169845117042314,-0.0329,0.015285));
#34698=CARTESIAN_POINT('',(0.0159522459658515,-0.0313489793100506,0.0153785797950748));
#34699=CARTESIAN_POINT('Ctrl Pts',(0.0159522459658615,-0.0313489793100606,
0.0153785797950649));
#34700=CARTESIAN_POINT('Ctrl Pts',(0.0160820906565023,-0.031415731059247,
0.0153780468914023));
#34701=CARTESIAN_POINT('Ctrl Pts',(0.0163106139035145,-0.0315359551043715,
0.0153768688374201));
#34702=CARTESIAN_POINT('',(0.0159577927381827,-0.03290000000001,0.0152429964807995));
#34703=CARTESIAN_POINT('Origin',(0.015285,-0.0329,0.0140154882957686));
#34704=CARTESIAN_POINT('Ctrl Pts',(0.0153785797950649,-0.0313489793100605,
0.0150477540341385));
#34705=CARTESIAN_POINT('Ctrl Pts',(0.0153780468914023,-0.031415731059247,
0.0149179093434977));
#34706=CARTESIAN_POINT('Ctrl Pts',(0.0153768688374201,-0.0315359551043715,
0.0146893860964855));
#34707=CARTESIAN_POINT('Origin',(0.0152429964808095,-0.0329,0.0159577927381728));
#34708=CARTESIAN_POINT('Ctrl Pts',(0.0153768688374201,-0.0315359551043715,
0.0163106139035145));
#34709=CARTESIAN_POINT('Ctrl Pts',(0.0153780468914023,-0.031415731059247,
0.0160820906565023));
#34710=CARTESIAN_POINT('Ctrl Pts',(0.0153785797950649,-0.0313489793100605,
0.0159522459658615));
#34711=CARTESIAN_POINT('Origin',(0.015715,-0.0329,0.0169845117042314));
#34712=CARTESIAN_POINT('',(0.0156214202049252,-0.0313489793100506,0.0159522459658515));
#34713=CARTESIAN_POINT('Ctrl Pts',(0.0156214202049351,-0.0313489793100605,
0.0159522459658615));
#34714=CARTESIAN_POINT('Ctrl Pts',(0.0156219531085977,-0.031415731059247,
0.0160820906565023));
#34715=CARTESIAN_POINT('Ctrl Pts',(0.0156231311625798,-0.0315359551043715,
0.0163106139035145));
#34716=CARTESIAN_POINT('',(0.0157570035192005,-0.03290000000001,0.0159577927381827));
#34717=CARTESIAN_POINT('Origin',(0.0157570035191905,-0.0329,0.0150422072618273));
#34718=CARTESIAN_POINT('',(0.0156214202049252,-0.0313489793100506,0.0150477540341485));
#34719=CARTESIAN_POINT('',(0.0157570035192005,-0.03290000000001,0.0150422072618173));
#34720=CARTESIAN_POINT('Ctrl Pts',(0.0156231311625798,-0.0315359551043715,
0.0146893860964855));
#34721=CARTESIAN_POINT('Ctrl Pts',(0.0156219531085977,-0.031415731059247,
0.0149179093434978));
#34722=CARTESIAN_POINT('Ctrl Pts',(0.0156214202049351,-0.0313489793100605,
0.0150477540341385));
#34723=CARTESIAN_POINT('Origin',(0.0159663575005511,-0.0329,0.0150336424994489));
#34724=CARTESIAN_POINT('Ctrl Pts',(0.0159522459658515,-0.0313489793100505,
0.0153785797950749));
#34725=CARTESIAN_POINT('Ctrl Pts',(0.015918774818534,-0.031331772155721,
0.0153787171660903));
#34726=CARTESIAN_POINT('Ctrl Pts',(0.0158847513530212,-0.0313150763778198,
0.0153736411394525));
#34727=CARTESIAN_POINT('Ctrl Pts',(0.0158307454010679,-0.0312913221771079,
0.015357513622913));
#34728=CARTESIAN_POINT('Ctrl Pts',(0.0158056188695749,-0.0312812420230617,
0.015347070513944));
#34729=CARTESIAN_POINT('Ctrl Pts',(0.0157580842126347,-0.0312670678991654,
0.015319217621804));
#34730=CARTESIAN_POINT('Ctrl Pts',(0.0157356483083034,-0.031263124157519,
0.0153017790139535));
#34731=CARTESIAN_POINT('Ctrl Pts',(0.0156982209860465,-0.031263124157519,
0.0152643516916966));
#34732=CARTESIAN_POINT('Ctrl Pts',(0.015680782378196,-0.0312670678991654,
0.0152419157873653));
#34733=CARTESIAN_POINT('Ctrl Pts',(0.015652929486056,-0.0312812420230617,
0.0151943811304251));
#34734=CARTESIAN_POINT('Ctrl Pts',(0.015642486377087,-0.0312913221771079,
0.0151692545989321));
#34735=CARTESIAN_POINT('Ctrl Pts',(0.0156263588605475,-0.0313150763778198,
0.0151152486469788));
#34736=CARTESIAN_POINT('Ctrl Pts',(0.0156212828339097,-0.031331772155721,
0.015081225181466));
#34737=CARTESIAN_POINT('Ctrl Pts',(0.0156214202049251,-0.0313489793100505,
0.0150477540341485));
#34738=CARTESIAN_POINT('Origin',(0.0159663575005511,-0.0329,0.0159663575005511));
#34739=CARTESIAN_POINT('',(0.0159522459658515,-0.0313489793100506,0.0156214202049252));
#34740=CARTESIAN_POINT('Ctrl Pts',(0.0156214202049251,-0.0313489793100505,
0.0159522459658515));
#34741=CARTESIAN_POINT('Ctrl Pts',(0.0156212828339097,-0.031331772155721,
0.015918774818534));
#34742=CARTESIAN_POINT('Ctrl Pts',(0.0156263588605475,-0.0313150763778198,
0.0158847513530212));
#34743=CARTESIAN_POINT('Ctrl Pts',(0.015642486377087,-0.0312913221771079,
0.0158307454010679));
#34744=CARTESIAN_POINT('Ctrl Pts',(0.015652929486056,-0.0312812420230617,
0.0158056188695749));
#34745=CARTESIAN_POINT('Ctrl Pts',(0.015680782378196,-0.0312670678991654,
0.0157580842126347));
#34746=CARTESIAN_POINT('Ctrl Pts',(0.0156982209860465,-0.031263124157519,
0.0157356483083034));
#34747=CARTESIAN_POINT('Ctrl Pts',(0.0157356483083034,-0.031263124157519,
0.0156982209860465));
#34748=CARTESIAN_POINT('Ctrl Pts',(0.0157580842126347,-0.0312670678991654,
0.015680782378196));
#34749=CARTESIAN_POINT('Ctrl Pts',(0.0158056188695749,-0.0312812420230617,
0.015652929486056));
#34750=CARTESIAN_POINT('Ctrl Pts',(0.0158307454010679,-0.0312913221771079,
0.015642486377087));
#34751=CARTESIAN_POINT('Ctrl Pts',(0.0158847513530212,-0.0313150763778198,
0.0156263588605475));
#34752=CARTESIAN_POINT('Ctrl Pts',(0.015918774818534,-0.031331772155721,
0.0156212828339097));
#34753=CARTESIAN_POINT('Ctrl Pts',(0.0159522459658515,-0.0313489793100505,
0.0156214202049251));
#34754=CARTESIAN_POINT('',(0.0159577927381827,-0.03290000000001,0.0157570035192005));
#34755=CARTESIAN_POINT('Origin',(0.0159577927381728,-0.0329,0.0157570035191905));
#34756=CARTESIAN_POINT('Ctrl Pts',(0.0163106139035145,-0.0315359551043715,
0.0156231311625798));
#34757=CARTESIAN_POINT('Ctrl Pts',(0.0160820906565023,-0.031415731059247,
0.0156219531085977));
#34758=CARTESIAN_POINT('Ctrl Pts',(0.0159522459658615,-0.0313489793100605,
0.0156214202049351));
#34759=CARTESIAN_POINT('Origin',(0.0155,-0.0313179775521807,0.0155));
#34760=CARTESIAN_POINT('',(0.0155,-0.0311,0.0155));
#34761=CARTESIAN_POINT('',(0.0159099561512377,-0.0313179775521807,0.0155));
#34762=CARTESIAN_POINT('Origin',(0.0155,-0.0301533625,0.0155));
#34763=CARTESIAN_POINT('',(0.016864685,-0.02980672499999,0.0155));
#34764=CARTESIAN_POINT('Origin',(0.01550000000001,-0.02980672499999,0.0155));
#34765=CARTESIAN_POINT('',(0.016864685,-0.0305,0.0155));
#34766=CARTESIAN_POINT('',(0.016864685,-0.0301533625,0.0155));
#34767=CARTESIAN_POINT('Origin',(0.01550000000001,-0.0305,0.0155));
#34768=CARTESIAN_POINT('Origin',(0.0134176575,-0.0305,0.0155));
#34769=CARTESIAN_POINT('Origin',(0.0155,-0.0296533625,0.0155));
#34770=CARTESIAN_POINT('',(0.0169323425,-0.0296533625,0.0155));
#34771=CARTESIAN_POINT('',(0.0583535235824775,0.254069413769245,0.0874146184444375));
#34772=CARTESIAN_POINT('',(0.0583535235824775,0.254069413769245,0.0874146184444375));
#34773=CARTESIAN_POINT('',(0.0583535235824775,0.254069413769245,0.0874146184444375));
#34774=CARTESIAN_POINT('',(0.0583535235824775,0.254069413769245,0.0874146184444375));
#34775=CARTESIAN_POINT('',(0.0583535235824775,0.254069413769245,0.0874146184444375));
#34776=CARTESIAN_POINT('',(0.0583535235824775,0.254069413769245,0.0874146184444375));
#34777=CARTESIAN_POINT('',(0.0583535235824826,0.25406941376924,0.0874146184444374));
#34778=CARTESIAN_POINT('',(0.0583535235824775,0.254069413769245,0.0874146184444375));
#34779=CARTESIAN_POINT('',(0.0583535235824775,0.254069413769245,0.0874146184444375));
#34780=CARTESIAN_POINT('',(0.0583535235824775,0.254069413769245,0.0874146184444375));
#34781=CARTESIAN_POINT('',(0.0583535235824775,0.254069413769245,0.0874146184444375));
#34782=CARTESIAN_POINT('',(0.0583535235824775,0.254069413769245,0.0874146184444375));
#34783=CARTESIAN_POINT('',(0.0583535235824775,0.254069413769245,0.0874146184444375));
#34784=CARTESIAN_POINT('',(0.0583535235824775,0.254069413769245,0.0874146184444375));
#34785=CARTESIAN_POINT('',(0.0583535235824775,0.254069413769245,0.0874146184444375));
#34786=CARTESIAN_POINT('',(0.0583535235824775,0.254069413769245,0.0874146184444375));
#34787=CARTESIAN_POINT('',(0.0583535235824775,0.254069413769245,0.0874146184444375));
#34788=CARTESIAN_POINT('',(0.0583535235824775,0.254069413769245,0.0874146184444375));
#34789=CARTESIAN_POINT('',(0.0583535235824775,0.254069413769245,0.0874146184444375));
#34790=CARTESIAN_POINT('',(0.0583535235824775,0.254069413769245,0.0874146184444375));
#34791=CARTESIAN_POINT('',(0.0583535235824775,0.254069413769245,0.0874146184444375));
#34792=CARTESIAN_POINT('',(0.0583535235824775,0.254069413769245,0.0874146184444375));
#34793=CARTESIAN_POINT('',(0.0583535235824775,0.254069413769245,0.0874146184444375));
#34794=CARTESIAN_POINT('',(0.0583535235824775,0.254069413769245,0.0874146184444375));
#34795=CARTESIAN_POINT('',(0.0583535235824775,0.254069413769245,0.0874146184444375));
#34796=CARTESIAN_POINT('',(0.0583535235824775,0.254069413769245,0.0874146184444375));
#34797=CARTESIAN_POINT('',(0.0583535235824775,0.254069413769245,0.0874146184444375));
#34798=CARTESIAN_POINT('',(0.0583535235824775,0.254069413769245,0.0874146184444375));
#34799=CARTESIAN_POINT('',(0.0583535235824775,0.254069413769245,0.0874146184444375));
#34800=CARTESIAN_POINT('',(0.0583535235824775,0.254069413769245,0.0874146184444375));
#34801=CARTESIAN_POINT('',(0.0583535235824775,0.254069413769245,0.0874146184444375));
#34802=CARTESIAN_POINT('',(0.0583535235824775,0.254069413769245,0.0874146184444375));
#34803=CARTESIAN_POINT('',(0.0583535235824775,0.254069413769245,0.0874146184444375));
#34804=CARTESIAN_POINT('',(0.0583359021125469,0.223051812309861,0.0874146184444474));
#34805=CARTESIAN_POINT('',(0.0893535235824875,0.254069413769255,0.0874146184444375));
#34806=CARTESIAN_POINT('',(0.0894139272636846,0.223130053767004,0.0874146184444374));
#34807=UNCERTAINTY_MEASURE_WITH_UNIT(LENGTH_MEASURE(1.E-5),#34877,
'DISTANCE_ACCURACY_VALUE',
'Maximum model space distance between geometric entities at asserted c
onnectivities');
#34808=UNCERTAINTY_MEASURE_WITH_UNIT(LENGTH_MEASURE(1.E-5),#34877,
'DISTANCE_ACCURACY_VALUE',
'Maximum model space distance between geometric entities at asserted c
onnectivities');
#34809=UNCERTAINTY_MEASURE_WITH_UNIT(LENGTH_MEASURE(1.E-5),#34877,
'DISTANCE_ACCURACY_VALUE',
'Maximum model space distance between geometric entities at asserted c
onnectivities');
#34810=UNCERTAINTY_MEASURE_WITH_UNIT(LENGTH_MEASURE(1.E-5),#34877,
'DISTANCE_ACCURACY_VALUE',
'Maximum model space distance between geometric entities at asserted c
onnectivities');
#34811=UNCERTAINTY_MEASURE_WITH_UNIT(LENGTH_MEASURE(1.E-5),#34877,
'DISTANCE_ACCURACY_VALUE',
'Maximum model space distance between geometric entities at asserted c
onnectivities');
#34812=UNCERTAINTY_MEASURE_WITH_UNIT(LENGTH_MEASURE(1.E-5),#34877,
'DISTANCE_ACCURACY_VALUE',
'Maximum model space distance between geometric entities at asserted c
onnectivities');
#34813=UNCERTAINTY_MEASURE_WITH_UNIT(LENGTH_MEASURE(1.E-5),#34877,
'DISTANCE_ACCURACY_VALUE',
'Maximum model space distance between geometric entities at asserted c
onnectivities');
#34814=UNCERTAINTY_MEASURE_WITH_UNIT(LENGTH_MEASURE(1.E-5),#34877,
'DISTANCE_ACCURACY_VALUE',
'Maximum model space distance between geometric entities at asserted c
onnectivities');
#34815=UNCERTAINTY_MEASURE_WITH_UNIT(LENGTH_MEASURE(1.E-5),#34877,
'DISTANCE_ACCURACY_VALUE',
'Maximum model space distance between geometric entities at asserted c
onnectivities');
#34816=UNCERTAINTY_MEASURE_WITH_UNIT(LENGTH_MEASURE(1.E-5),#34877,
'DISTANCE_ACCURACY_VALUE',
'Maximum model space distance between geometric entities at asserted c
onnectivities');
#34817=UNCERTAINTY_MEASURE_WITH_UNIT(LENGTH_MEASURE(1.E-5),#34877,
'DISTANCE_ACCURACY_VALUE',
'Maximum model space distance between geometric entities at asserted c
onnectivities');
#34818=UNCERTAINTY_MEASURE_WITH_UNIT(LENGTH_MEASURE(1.E-5),#34877,
'DISTANCE_ACCURACY_VALUE',
'Maximum model space distance between geometric entities at asserted c
onnectivities');
#34819=UNCERTAINTY_MEASURE_WITH_UNIT(LENGTH_MEASURE(1.E-5),#34877,
'DISTANCE_ACCURACY_VALUE',
'Maximum model space distance between geometric entities at asserted c
onnectivities');
#34820=UNCERTAINTY_MEASURE_WITH_UNIT(LENGTH_MEASURE(1.E-5),#34877,
'DISTANCE_ACCURACY_VALUE',
'Maximum model space distance between geometric entities at asserted c
onnectivities');
#34821=UNCERTAINTY_MEASURE_WITH_UNIT(LENGTH_MEASURE(1.E-5),#34877,
'DISTANCE_ACCURACY_VALUE',
'Maximum model space distance between geometric entities at asserted c
onnectivities');
#34822=UNCERTAINTY_MEASURE_WITH_UNIT(LENGTH_MEASURE(1.E-5),#34877,
'DISTANCE_ACCURACY_VALUE',
'Maximum model space distance between geometric entities at asserted c
onnectivities');
#34823=UNCERTAINTY_MEASURE_WITH_UNIT(LENGTH_MEASURE(1.E-5),#34877,
'DISTANCE_ACCURACY_VALUE',
'Maximum model space distance between geometric entities at asserted c
onnectivities');
#34824=UNCERTAINTY_MEASURE_WITH_UNIT(LENGTH_MEASURE(1.E-5),#34877,
'DISTANCE_ACCURACY_VALUE',
'Maximum model space distance between geometric entities at asserted c
onnectivities');
#34825=UNCERTAINTY_MEASURE_WITH_UNIT(LENGTH_MEASURE(1.E-5),#34877,
'DISTANCE_ACCURACY_VALUE',
'Maximum model space distance between geometric entities at asserted c
onnectivities');
#34826=UNCERTAINTY_MEASURE_WITH_UNIT(LENGTH_MEASURE(1.E-5),#34877,
'DISTANCE_ACCURACY_VALUE',
'Maximum model space distance between geometric entities at asserted c
onnectivities');
#34827=UNCERTAINTY_MEASURE_WITH_UNIT(LENGTH_MEASURE(1.E-5),#34877,
'DISTANCE_ACCURACY_VALUE',
'Maximum model space distance between geometric entities at asserted c
onnectivities');
#34828=UNCERTAINTY_MEASURE_WITH_UNIT(LENGTH_MEASURE(1.E-5),#34877,
'DISTANCE_ACCURACY_VALUE',
'Maximum model space distance between geometric entities at asserted c
onnectivities');
#34829=UNCERTAINTY_MEASURE_WITH_UNIT(LENGTH_MEASURE(1.E-5),#34877,
'DISTANCE_ACCURACY_VALUE',
'Maximum model space distance between geometric entities at asserted c
onnectivities');
#34830=UNCERTAINTY_MEASURE_WITH_UNIT(LENGTH_MEASURE(1.E-5),#34877,
'DISTANCE_ACCURACY_VALUE',
'Maximum model space distance between geometric entities at asserted c
onnectivities');
#34831=UNCERTAINTY_MEASURE_WITH_UNIT(LENGTH_MEASURE(1.E-5),#34877,
'DISTANCE_ACCURACY_VALUE',
'Maximum model space distance between geometric entities at asserted c
onnectivities');
#34832=UNCERTAINTY_MEASURE_WITH_UNIT(LENGTH_MEASURE(1.E-5),#34877,
'DISTANCE_ACCURACY_VALUE',
'Maximum model space distance between geometric entities at asserted c
onnectivities');
#34833=UNCERTAINTY_MEASURE_WITH_UNIT(LENGTH_MEASURE(1.E-5),#34877,
'DISTANCE_ACCURACY_VALUE',
'Maximum model space distance between geometric entities at asserted c
onnectivities');
#34834=UNCERTAINTY_MEASURE_WITH_UNIT(LENGTH_MEASURE(1.E-5),#34877,
'DISTANCE_ACCURACY_VALUE',
'Maximum model space distance between geometric entities at asserted c
onnectivities');
#34835=UNCERTAINTY_MEASURE_WITH_UNIT(LENGTH_MEASURE(1.E-5),#34877,
'DISTANCE_ACCURACY_VALUE',
'Maximum model space distance between geometric entities at asserted c
onnectivities');
#34836=UNCERTAINTY_MEASURE_WITH_UNIT(LENGTH_MEASURE(1.E-5),#34877,
'DISTANCE_ACCURACY_VALUE',
'Maximum model space distance between geometric entities at asserted c
onnectivities');
#34837=UNCERTAINTY_MEASURE_WITH_UNIT(LENGTH_MEASURE(1.E-5),#34877,
'DISTANCE_ACCURACY_VALUE',
'Maximum model space distance between geometric entities at asserted c
onnectivities');
#34838=UNCERTAINTY_MEASURE_WITH_UNIT(LENGTH_MEASURE(1.E-5),#34877,
'DISTANCE_ACCURACY_VALUE',
'Maximum model space distance between geometric entities at asserted c
onnectivities');
#34839=UNCERTAINTY_MEASURE_WITH_UNIT(LENGTH_MEASURE(1.E-5),#34877,
'DISTANCE_ACCURACY_VALUE',
'Maximum model space distance between geometric entities at asserted c
onnectivities');
#34840=UNCERTAINTY_MEASURE_WITH_UNIT(LENGTH_MEASURE(1.E-5),#34877,
'DISTANCE_ACCURACY_VALUE',
'Maximum model space distance between geometric entities at asserted c
onnectivities');
#34841=UNCERTAINTY_MEASURE_WITH_UNIT(LENGTH_MEASURE(1.E-5),#34877,
'DISTANCE_ACCURACY_VALUE',
'Maximum model space distance between geometric entities at asserted c
onnectivities');
#34842=(
GEOMETRIC_REPRESENTATION_CONTEXT(3)
GLOBAL_UNCERTAINTY_ASSIGNED_CONTEXT((#34807))
GLOBAL_UNIT_ASSIGNED_CONTEXT((#34877,#34878,#34879))
REPRESENTATION_CONTEXT('','3D')
);
#34843=(
GEOMETRIC_REPRESENTATION_CONTEXT(3)
GLOBAL_UNCERTAINTY_ASSIGNED_CONTEXT((#34808))
GLOBAL_UNIT_ASSIGNED_CONTEXT((#34877,#34878,#34879))
REPRESENTATION_CONTEXT('','3D')
);
#34844=(
GEOMETRIC_REPRESENTATION_CONTEXT(3)
GLOBAL_UNCERTAINTY_ASSIGNED_CONTEXT((#34809))
GLOBAL_UNIT_ASSIGNED_CONTEXT((#34877,#34878,#34879))
REPRESENTATION_CONTEXT('','3D')
);
#34845=(
GEOMETRIC_REPRESENTATION_CONTEXT(3)
GLOBAL_UNCERTAINTY_ASSIGNED_CONTEXT((#34810))
GLOBAL_UNIT_ASSIGNED_CONTEXT((#34877,#34878,#34879))
REPRESENTATION_CONTEXT('','3D')
);
#34846=(
GEOMETRIC_REPRESENTATION_CONTEXT(3)
GLOBAL_UNCERTAINTY_ASSIGNED_CONTEXT((#34811))
GLOBAL_UNIT_ASSIGNED_CONTEXT((#34877,#34878,#34879))
REPRESENTATION_CONTEXT('','3D')
);
#34847=(
GEOMETRIC_REPRESENTATION_CONTEXT(3)
GLOBAL_UNCERTAINTY_ASSIGNED_CONTEXT((#34812))
GLOBAL_UNIT_ASSIGNED_CONTEXT((#34877,#34878,#34879))
REPRESENTATION_CONTEXT('','3D')
);
#34848=(
GEOMETRIC_REPRESENTATION_CONTEXT(3)
GLOBAL_UNCERTAINTY_ASSIGNED_CONTEXT((#34813))
GLOBAL_UNIT_ASSIGNED_CONTEXT((#34877,#34878,#34879))
REPRESENTATION_CONTEXT('','3D')
);
#34849=(
GEOMETRIC_REPRESENTATION_CONTEXT(3)
GLOBAL_UNCERTAINTY_ASSIGNED_CONTEXT((#34814))
GLOBAL_UNIT_ASSIGNED_CONTEXT((#34877,#34878,#34879))
REPRESENTATION_CONTEXT('','3D')
);
#34850=(
GEOMETRIC_REPRESENTATION_CONTEXT(3)
GLOBAL_UNCERTAINTY_ASSIGNED_CONTEXT((#34815))
GLOBAL_UNIT_ASSIGNED_CONTEXT((#34877,#34878,#34879))
REPRESENTATION_CONTEXT('','3D')
);
#34851=(
GEOMETRIC_REPRESENTATION_CONTEXT(3)
GLOBAL_UNCERTAINTY_ASSIGNED_CONTEXT((#34816))
GLOBAL_UNIT_ASSIGNED_CONTEXT((#34877,#34878,#34879))
REPRESENTATION_CONTEXT('','3D')
);
#34852=(
GEOMETRIC_REPRESENTATION_CONTEXT(3)
GLOBAL_UNCERTAINTY_ASSIGNED_CONTEXT((#34817))
GLOBAL_UNIT_ASSIGNED_CONTEXT((#34877,#34878,#34879))
REPRESENTATION_CONTEXT('','3D')
);
#34853=(
GEOMETRIC_REPRESENTATION_CONTEXT(3)
GLOBAL_UNCERTAINTY_ASSIGNED_CONTEXT((#34818))
GLOBAL_UNIT_ASSIGNED_CONTEXT((#34877,#34878,#34879))
REPRESENTATION_CONTEXT('','3D')
);
#34854=(
GEOMETRIC_REPRESENTATION_CONTEXT(3)
GLOBAL_UNCERTAINTY_ASSIGNED_CONTEXT((#34819))
GLOBAL_UNIT_ASSIGNED_CONTEXT((#34877,#34878,#34879))
REPRESENTATION_CONTEXT('','3D')
);
#34855=(
GEOMETRIC_REPRESENTATION_CONTEXT(3)
GLOBAL_UNCERTAINTY_ASSIGNED_CONTEXT((#34820))
GLOBAL_UNIT_ASSIGNED_CONTEXT((#34877,#34878,#34879))
REPRESENTATION_CONTEXT('','3D')
);
#34856=(
GEOMETRIC_REPRESENTATION_CONTEXT(3)
GLOBAL_UNCERTAINTY_ASSIGNED_CONTEXT((#34821))
GLOBAL_UNIT_ASSIGNED_CONTEXT((#34877,#34878,#34879))
REPRESENTATION_CONTEXT('','3D')
);
#34857=(
GEOMETRIC_REPRESENTATION_CONTEXT(3)
GLOBAL_UNCERTAINTY_ASSIGNED_CONTEXT((#34822))
GLOBAL_UNIT_ASSIGNED_CONTEXT((#34877,#34878,#34879))
REPRESENTATION_CONTEXT('','3D')
);
#34858=(
GEOMETRIC_REPRESENTATION_CONTEXT(3)
GLOBAL_UNCERTAINTY_ASSIGNED_CONTEXT((#34823))
GLOBAL_UNIT_ASSIGNED_CONTEXT((#34877,#34878,#34879))
REPRESENTATION_CONTEXT('','3D')
);
#34859=(
GEOMETRIC_REPRESENTATION_CONTEXT(3)
GLOBAL_UNCERTAINTY_ASSIGNED_CONTEXT((#34824))
GLOBAL_UNIT_ASSIGNED_CONTEXT((#34877,#34878,#34879))
REPRESENTATION_CONTEXT('','3D')
);
#34860=(
GEOMETRIC_REPRESENTATION_CONTEXT(3)
GLOBAL_UNCERTAINTY_ASSIGNED_CONTEXT((#34825))
GLOBAL_UNIT_ASSIGNED_CONTEXT((#34877,#34878,#34879))
REPRESENTATION_CONTEXT('','3D')
);
#34861=(
GEOMETRIC_REPRESENTATION_CONTEXT(3)
GLOBAL_UNCERTAINTY_ASSIGNED_CONTEXT((#34826))
GLOBAL_UNIT_ASSIGNED_CONTEXT((#34877,#34878,#34879))
REPRESENTATION_CONTEXT('','3D')
);
#34862=(
GEOMETRIC_REPRESENTATION_CONTEXT(3)
GLOBAL_UNCERTAINTY_ASSIGNED_CONTEXT((#34827))
GLOBAL_UNIT_ASSIGNED_CONTEXT((#34877,#34878,#34879))
REPRESENTATION_CONTEXT('','3D')
);
#34863=(
GEOMETRIC_REPRESENTATION_CONTEXT(3)
GLOBAL_UNCERTAINTY_ASSIGNED_CONTEXT((#34828))
GLOBAL_UNIT_ASSIGNED_CONTEXT((#34877,#34878,#34879))
REPRESENTATION_CONTEXT('','3D')
);
#34864=(
GEOMETRIC_REPRESENTATION_CONTEXT(3)
GLOBAL_UNCERTAINTY_ASSIGNED_CONTEXT((#34829))
GLOBAL_UNIT_ASSIGNED_CONTEXT((#34877,#34878,#34879))
REPRESENTATION_CONTEXT('','3D')
);
#34865=(
GEOMETRIC_REPRESENTATION_CONTEXT(3)
GLOBAL_UNCERTAINTY_ASSIGNED_CONTEXT((#34830))
GLOBAL_UNIT_ASSIGNED_CONTEXT((#34877,#34878,#34879))
REPRESENTATION_CONTEXT('','3D')
);
#34866=(
GEOMETRIC_REPRESENTATION_CONTEXT(3)
GLOBAL_UNCERTAINTY_ASSIGNED_CONTEXT((#34831))
GLOBAL_UNIT_ASSIGNED_CONTEXT((#34877,#34878,#34879))
REPRESENTATION_CONTEXT('','3D')
);
#34867=(
GEOMETRIC_REPRESENTATION_CONTEXT(3)
GLOBAL_UNCERTAINTY_ASSIGNED_CONTEXT((#34832))
GLOBAL_UNIT_ASSIGNED_CONTEXT((#34877,#34878,#34879))
REPRESENTATION_CONTEXT('','3D')
);
#34868=(
GEOMETRIC_REPRESENTATION_CONTEXT(3)
GLOBAL_UNCERTAINTY_ASSIGNED_CONTEXT((#34833))
GLOBAL_UNIT_ASSIGNED_CONTEXT((#34877,#34878,#34879))
REPRESENTATION_CONTEXT('','3D')
);
#34869=(
GEOMETRIC_REPRESENTATION_CONTEXT(3)
GLOBAL_UNCERTAINTY_ASSIGNED_CONTEXT((#34834))
GLOBAL_UNIT_ASSIGNED_CONTEXT((#34877,#34878,#34879))
REPRESENTATION_CONTEXT('','3D')
);
#34870=(
GEOMETRIC_REPRESENTATION_CONTEXT(3)
GLOBAL_UNCERTAINTY_ASSIGNED_CONTEXT((#34835))
GLOBAL_UNIT_ASSIGNED_CONTEXT((#34877,#34878,#34879))
REPRESENTATION_CONTEXT('','3D')
);
#34871=(
GEOMETRIC_REPRESENTATION_CONTEXT(3)
GLOBAL_UNCERTAINTY_ASSIGNED_CONTEXT((#34836))
GLOBAL_UNIT_ASSIGNED_CONTEXT((#34877,#34878,#34879))
REPRESENTATION_CONTEXT('','3D')
);
#34872=(
GEOMETRIC_REPRESENTATION_CONTEXT(3)
GLOBAL_UNCERTAINTY_ASSIGNED_CONTEXT((#34837))
GLOBAL_UNIT_ASSIGNED_CONTEXT((#34877,#34878,#34879))
REPRESENTATION_CONTEXT('','3D')
);
#34873=(
GEOMETRIC_REPRESENTATION_CONTEXT(3)
GLOBAL_UNCERTAINTY_ASSIGNED_CONTEXT((#34838))
GLOBAL_UNIT_ASSIGNED_CONTEXT((#34877,#34878,#34879))
REPRESENTATION_CONTEXT('','3D')
);
#34874=(
GEOMETRIC_REPRESENTATION_CONTEXT(3)
GLOBAL_UNCERTAINTY_ASSIGNED_CONTEXT((#34839))
GLOBAL_UNIT_ASSIGNED_CONTEXT((#34877,#34878,#34879))
REPRESENTATION_CONTEXT('','3D')
);
#34875=(
GEOMETRIC_REPRESENTATION_CONTEXT(3)
GLOBAL_UNCERTAINTY_ASSIGNED_CONTEXT((#34840))
GLOBAL_UNIT_ASSIGNED_CONTEXT((#34877,#34878,#34879))
REPRESENTATION_CONTEXT('','3D')
);
#34876=(
GEOMETRIC_REPRESENTATION_CONTEXT(3)
GLOBAL_UNCERTAINTY_ASSIGNED_CONTEXT((#34841))
GLOBAL_UNIT_ASSIGNED_CONTEXT((#34877,#34878,#34879))
REPRESENTATION_CONTEXT('','3D')
);
#34877=(
LENGTH_UNIT()
NAMED_UNIT(*)
SI_UNIT($,.METRE.)
);
#34878=(
NAMED_UNIT(*)
PLANE_ANGLE_UNIT()
SI_UNIT($,.RADIAN.)
);
#34879=(
NAMED_UNIT(*)
SI_UNIT($,.STERADIAN.)
SOLID_ANGLE_UNIT()
);
#34880=SHAPE_DEFINITION_REPRESENTATION(#34914,#34984);
#34881=SHAPE_DEFINITION_REPRESENTATION(#34915,#34985);
#34882=SHAPE_DEFINITION_REPRESENTATION(#34916,#34986);
#34883=SHAPE_DEFINITION_REPRESENTATION(#34917,#34987);
#34884=SHAPE_DEFINITION_REPRESENTATION(#34918,#34988);
#34885=SHAPE_DEFINITION_REPRESENTATION(#34919,#34989);
#34886=SHAPE_DEFINITION_REPRESENTATION(#34920,#34990);
#34887=SHAPE_DEFINITION_REPRESENTATION(#34921,#34991);
#34888=SHAPE_DEFINITION_REPRESENTATION(#34922,#34992);
#34889=SHAPE_DEFINITION_REPRESENTATION(#34923,#34993);
#34890=SHAPE_DEFINITION_REPRESENTATION(#34924,#34994);
#34891=SHAPE_DEFINITION_REPRESENTATION(#34925,#34995);
#34892=SHAPE_DEFINITION_REPRESENTATION(#34926,#34996);
#34893=SHAPE_DEFINITION_REPRESENTATION(#34927,#34997);
#34894=SHAPE_DEFINITION_REPRESENTATION(#34928,#34998);
#34895=SHAPE_DEFINITION_REPRESENTATION(#34929,#34999);
#34896=SHAPE_DEFINITION_REPRESENTATION(#34930,#35000);
#34897=SHAPE_DEFINITION_REPRESENTATION(#34931,#35001);
#34898=SHAPE_DEFINITION_REPRESENTATION(#34932,#35002);
#34899=SHAPE_DEFINITION_REPRESENTATION(#34933,#35003);
#34900=SHAPE_DEFINITION_REPRESENTATION(#34934,#35004);
#34901=SHAPE_DEFINITION_REPRESENTATION(#34935,#35005);
#34902=SHAPE_DEFINITION_REPRESENTATION(#34936,#35006);
#34903=SHAPE_DEFINITION_REPRESENTATION(#34937,#35007);
#34904=SHAPE_DEFINITION_REPRESENTATION(#34938,#35008);
#34905=SHAPE_DEFINITION_REPRESENTATION(#34939,#35009);
#34906=SHAPE_DEFINITION_REPRESENTATION(#34940,#35010);
#34907=SHAPE_DEFINITION_REPRESENTATION(#34941,#35011);
#34908=SHAPE_DEFINITION_REPRESENTATION(#34942,#35012);
#34909=SHAPE_DEFINITION_REPRESENTATION(#34943,#35013);
#34910=SHAPE_DEFINITION_REPRESENTATION(#34944,#35014);
#34911=SHAPE_DEFINITION_REPRESENTATION(#34945,#35015);
#34912=SHAPE_DEFINITION_REPRESENTATION(#34946,#35016);
#34913=SHAPE_DEFINITION_REPRESENTATION(#34947,#35017);
#34914=PRODUCT_DEFINITION_SHAPE('',$,#35019);
#34915=PRODUCT_DEFINITION_SHAPE('',$,#35020);
#34916=PRODUCT_DEFINITION_SHAPE('',$,#35021);
#34917=PRODUCT_DEFINITION_SHAPE('',$,#35022);
#34918=PRODUCT_DEFINITION_SHAPE('',$,#35023);
#34919=PRODUCT_DEFINITION_SHAPE('',$,#35024);
#34920=PRODUCT_DEFINITION_SHAPE('',$,#35025);
#34921=PRODUCT_DEFINITION_SHAPE('',$,#35026);
#34922=PRODUCT_DEFINITION_SHAPE('',$,#35027);
#34923=PRODUCT_DEFINITION_SHAPE('',$,#35028);
#34924=PRODUCT_DEFINITION_SHAPE('',$,#35029);
#34925=PRODUCT_DEFINITION_SHAPE('',$,#35030);
#34926=PRODUCT_DEFINITION_SHAPE('',$,#35031);
#34927=PRODUCT_DEFINITION_SHAPE('',$,#35032);
#34928=PRODUCT_DEFINITION_SHAPE('',$,#35033);
#34929=PRODUCT_DEFINITION_SHAPE('',$,#35034);
#34930=PRODUCT_DEFINITION_SHAPE('',$,#35035);
#34931=PRODUCT_DEFINITION_SHAPE('',$,#35036);
#34932=PRODUCT_DEFINITION_SHAPE('',$,#35037);
#34933=PRODUCT_DEFINITION_SHAPE('',$,#35038);
#34934=PRODUCT_DEFINITION_SHAPE('',$,#35039);
#34935=PRODUCT_DEFINITION_SHAPE('',$,#35040);
#34936=PRODUCT_DEFINITION_SHAPE('',$,#35041);
#34937=PRODUCT_DEFINITION_SHAPE('',$,#35042);
#34938=PRODUCT_DEFINITION_SHAPE('',$,#35043);
#34939=PRODUCT_DEFINITION_SHAPE('',$,#35044);
#34940=PRODUCT_DEFINITION_SHAPE('',$,#35045);
#34941=PRODUCT_DEFINITION_SHAPE('',$,#35046);
#34942=PRODUCT_DEFINITION_SHAPE('',$,#35047);
#34943=PRODUCT_DEFINITION_SHAPE('',$,#35048);
#34944=PRODUCT_DEFINITION_SHAPE('',$,#35049);
#34945=PRODUCT_DEFINITION_SHAPE('',$,#35050);
#34946=PRODUCT_DEFINITION_SHAPE('',$,#35051);
#34947=PRODUCT_DEFINITION_SHAPE('',$,#35052);
#34948=PRODUCT_DEFINITION_SHAPE($,$,#119);
#34949=PRODUCT_DEFINITION_SHAPE($,$,#120);
#34950=PRODUCT_DEFINITION_SHAPE($,$,#121);
#34951=PRODUCT_DEFINITION_SHAPE($,$,#122);
#34952=PRODUCT_DEFINITION_SHAPE($,$,#123);
#34953=PRODUCT_DEFINITION_SHAPE($,$,#124);
#34954=PRODUCT_DEFINITION_SHAPE($,$,#125);
#34955=PRODUCT_DEFINITION_SHAPE($,$,#126);
#34956=PRODUCT_DEFINITION_SHAPE($,$,#127);
#34957=PRODUCT_DEFINITION_SHAPE($,$,#128);
#34958=PRODUCT_DEFINITION_SHAPE($,$,#129);
#34959=PRODUCT_DEFINITION_SHAPE($,$,#130);
#34960=PRODUCT_DEFINITION_SHAPE($,$,#131);
#34961=PRODUCT_DEFINITION_SHAPE($,$,#132);
#34962=PRODUCT_DEFINITION_SHAPE($,$,#133);
#34963=PRODUCT_DEFINITION_SHAPE($,$,#134);
#34964=PRODUCT_DEFINITION_SHAPE($,$,#135);
#34965=PRODUCT_DEFINITION_SHAPE($,$,#136);
#34966=PRODUCT_DEFINITION_SHAPE($,$,#137);
#34967=PRODUCT_DEFINITION_SHAPE($,$,#138);
#34968=PRODUCT_DEFINITION_SHAPE($,$,#139);
#34969=PRODUCT_DEFINITION_SHAPE($,$,#140);
#34970=PRODUCT_DEFINITION_SHAPE($,$,#141);
#34971=PRODUCT_DEFINITION_SHAPE($,$,#142);
#34972=PRODUCT_DEFINITION_SHAPE($,$,#143);
#34973=PRODUCT_DEFINITION_SHAPE($,$,#144);
#34974=PRODUCT_DEFINITION_SHAPE($,$,#145);
#34975=PRODUCT_DEFINITION_SHAPE($,$,#146);
#34976=PRODUCT_DEFINITION_SHAPE($,$,#147);
#34977=PRODUCT_DEFINITION_SHAPE($,$,#148);
#34978=PRODUCT_DEFINITION_SHAPE($,$,#149);
#34979=PRODUCT_DEFINITION_SHAPE($,$,#150);
#34980=PRODUCT_DEFINITION_SHAPE($,$,#151);
#34981=PRODUCT_DEFINITION_SHAPE($,$,#152);
#34982=PRODUCT_DEFINITION_SHAPE($,$,#153);
#34983=PRODUCT_DEFINITION_SHAPE($,$,#154);
#34984=SHAPE_REPRESENTATION('',(#19951,#22222,#22223,#22224,#22225,#22226,
#22227,#22228,#22229,#22230,#22231,#22232,#22233,#22234,#22235,#22236,#22237,
#22238,#22239,#22240,#22241,#22242,#22243,#22244,#22245,#22246,#22247,#22248,
#22249,#22250,#22251,#22252,#22253,#22254,#22255,#22256,#22257),#34842);
#34985=SHAPE_REPRESENTATION('',(#19952),#34843);
#34986=SHAPE_REPRESENTATION('',(#19969),#34844);
#34987=SHAPE_REPRESENTATION('',(#20050),#34845);
#34988=SHAPE_REPRESENTATION('',(#20059),#34846);
#34989=SHAPE_REPRESENTATION('',(#20315),#34847);
#34990=SHAPE_REPRESENTATION('',(#20591),#34848);
#34991=SHAPE_REPRESENTATION('',(#20792),#34849);
#34992=SHAPE_REPRESENTATION('',(#20809),#34850);
#34993=SHAPE_REPRESENTATION('',(#20821),#34851);
#34994=SHAPE_REPRESENTATION('',(#20833),#34852);
#34995=SHAPE_REPRESENTATION('',(#20884),#34853);
#34996=SHAPE_REPRESENTATION('',(#20965),#34854);
#34997=SHAPE_REPRESENTATION('',(#21089),#34855);
#34998=SHAPE_REPRESENTATION('',(#21170),#34856);
#34999=SHAPE_REPRESENTATION('',(#21196),#34857);
#35000=SHAPE_REPRESENTATION('',(#21215),#34858);
#35001=SHAPE_REPRESENTATION('',(#21260),#34859);
#35002=SHAPE_REPRESENTATION('',(#21272),#34860);
#35003=SHAPE_REPRESENTATION('',(#21353),#34861);
#35004=SHAPE_REPRESENTATION('',(#21362),#34862);
#35005=SHAPE_REPRESENTATION('',(#21374),#34863);
#35006=SHAPE_REPRESENTATION('',(#21650),#34864);
#35007=SHAPE_REPRESENTATION('',(#21667),#34865);
#35008=SHAPE_REPRESENTATION('',(#21748),#34866);
#35009=SHAPE_REPRESENTATION('',(#21760),#34867);
#35010=SHAPE_REPRESENTATION('',(#21823),#34868);
#35011=SHAPE_REPRESENTATION('',(#21904),#34869);
#35012=SHAPE_REPRESENTATION('',(#21959),#34870);
#35013=SHAPE_REPRESENTATION('',(#21968),#34871);
#35014=SHAPE_REPRESENTATION('',(#22049),#34872);
#35015=SHAPE_REPRESENTATION('',(#22130),#34873);
#35016=SHAPE_REPRESENTATION('',(#22147),#34874);
#35017=SHAPE_REPRESENTATION('',(#22159),#34875);
#35018=PRODUCT_DEFINITION_CONTEXT('part definition',#35122,'design');
#35019=PRODUCT_DEFINITION('Stepper Motor Reference Model',
'MAT-073',#35053,#35018);
#35020=PRODUCT_DEFINITION('Interface component A',
'Interface component A',#35054,#35018);
#35021=PRODUCT_DEFINITION('Motor Stator Face 1','Motor Stator Face 1',#35055,
#35018);
#35022=PRODUCT_DEFINITION('Motor Plastic Spacer Right',
'Motor Plastic Spacer Right',#35056,#35018);
#35023=PRODUCT_DEFINITION('Motor Plastic Cover 1',
'Motor Plastic Cover 1',#35057,#35018);
#35024=PRODUCT_DEFINITION('Motor Shaft 1','Motor Shaft 1',#35058,#35018);
#35025=PRODUCT_DEFINITION('Motor Base Cap','Motor Base Cap',#35059,#35018);
#35026=PRODUCT_DEFINITION('Interface component D',
'Interface component D',#35060,#35018);
#35027=PRODUCT_DEFINITION('Socket Screw 1','Socket Screw 1',#35061,#35018);
#35028=PRODUCT_DEFINITION('Socket Screw 2','Socket Screw 2',#35062,#35018);
#35029=PRODUCT_DEFINITION('External Shaft Retaining Ring Clip',
'External Shaft Retaining Ring Clip',#35063,#35018);
#35030=PRODUCT_DEFINITION('Motor Stator Face 2','Motor Stator Face 2',#35064,
#35018);
#35031=PRODUCT_DEFINITION('Motor Top Cap','Motor Top Cap',#35065,#35018);
#35032=PRODUCT_DEFINITION('Motor Stator Face 3','Motor Stator Face 3',#35066,
#35018);
#35033=PRODUCT_DEFINITION('Motor Shaft 2','Motor Shaft 2',#35067,#35018);
#35034=PRODUCT_DEFINITION('Motor Plastic Protector',
'Motor Plastic Protector',#35068,#35018);
#35035=PRODUCT_DEFINITION('Motor PCB','Motor PCB',#35069,#35018);
#35036=PRODUCT_DEFINITION('Socket Screw 3','Socket Screw 3',#35070,#35018);
#35037=PRODUCT_DEFINITION('Motor Stator Face 4','Motor Stator Face 4',#35071,
#35018);
#35038=PRODUCT_DEFINITION('Motor Plastic Spacer Left',
'Motor Plastic Spacer Left',#35072,#35018);
#35039=PRODUCT_DEFINITION('Socket Screw 4','Socket Screw 4',#35073,#35018);
#35040=PRODUCT_DEFINITION('Motor Shaft 3','Motor Shaft 3',#35074,#35018);
#35041=PRODUCT_DEFINITION('Interface component B',
'Interface component B',#35075,#35018);
#35042=PRODUCT_DEFINITION('Motor Stator Face 5','Motor Stator Face 5',#35076,
#35018);
#35043=PRODUCT_DEFINITION('Socket Screw 5','Socket Screw 5',#35077,#35018);
#35044=PRODUCT_DEFINITION('Motor Central Spacer','Motor Central Spacer',
#35078,#35018);
#35045=PRODUCT_DEFINITION('Motor Stator Face 6','Motor Stator Face 6',#35079,
#35018);
#35046=PRODUCT_DEFINITION('Socket Screw 6','Socket Screw 6',#35080,#35018);
#35047=PRODUCT_DEFINITION('Motor Shaft 4','Motor Shaft 4',#35081,#35018);
#35048=PRODUCT_DEFINITION('Motor Stator Face 7','Motor Stator Face 7',#35082,
#35018);
#35049=PRODUCT_DEFINITION('Motor Stator Face 8','Motor Stator Face 8',#35083,
#35018);
#35050=PRODUCT_DEFINITION('Interface component C',
'Interface component C',#35084,#35018);
#35051=PRODUCT_DEFINITION('Socket Screw 7','Socket Screw 7',#35085,#35018);
#35052=PRODUCT_DEFINITION('Pan Head Screw M3x25 1',
'Pan Head Screw M3x25 1',#35086,#35018);
#35053=PRODUCT_DEFINITION_FORMATION('',$,#35124);
#35054=PRODUCT_DEFINITION_FORMATION('',$,#35125);
#35055=PRODUCT_DEFINITION_FORMATION('',$,#35126);
#35056=PRODUCT_DEFINITION_FORMATION('',$,#35127);
#35057=PRODUCT_DEFINITION_FORMATION('',$,#35128);
#35058=PRODUCT_DEFINITION_FORMATION('',$,#35129);
#35059=PRODUCT_DEFINITION_FORMATION('',$,#35130);
#35060=PRODUCT_DEFINITION_FORMATION('',$,#35131);
#35061=PRODUCT_DEFINITION_FORMATION('',$,#35132);
#35062=PRODUCT_DEFINITION_FORMATION('',$,#35133);
#35063=PRODUCT_DEFINITION_FORMATION('',$,#35134);
#35064=PRODUCT_DEFINITION_FORMATION('',$,#35135);
#35065=PRODUCT_DEFINITION_FORMATION('',$,#35136);
#35066=PRODUCT_DEFINITION_FORMATION('',$,#35137);
#35067=PRODUCT_DEFINITION_FORMATION('',$,#35138);
#35068=PRODUCT_DEFINITION_FORMATION('',$,#35139);
#35069=PRODUCT_DEFINITION_FORMATION('',$,#35140);
#35070=PRODUCT_DEFINITION_FORMATION('',$,#35141);
#35071=PRODUCT_DEFINITION_FORMATION('',$,#35142);
#35072=PRODUCT_DEFINITION_FORMATION('',$,#35143);
#35073=PRODUCT_DEFINITION_FORMATION('',$,#35144);
#35074=PRODUCT_DEFINITION_FORMATION('',$,#35145);
#35075=PRODUCT_DEFINITION_FORMATION('',$,#35146);
#35076=PRODUCT_DEFINITION_FORMATION('',$,#35147);
#35077=PRODUCT_DEFINITION_FORMATION('',$,#35148);
#35078=PRODUCT_DEFINITION_FORMATION('',$,#35149);
#35079=PRODUCT_DEFINITION_FORMATION('',$,#35150);
#35080=PRODUCT_DEFINITION_FORMATION('',$,#35151);
#35081=PRODUCT_DEFINITION_FORMATION('',$,#35152);
#35082=PRODUCT_DEFINITION_FORMATION('',$,#35153);
#35083=PRODUCT_DEFINITION_FORMATION('',$,#35154);
#35084=PRODUCT_DEFINITION_FORMATION('',$,#35155);
#35085=PRODUCT_DEFINITION_FORMATION('',$,#35156);
#35086=PRODUCT_DEFINITION_FORMATION('',$,#35157);
#35087=PRODUCT_RELATED_PRODUCT_CATEGORY(
'MAT-073','MAT-073',(#35124));
#35088=PRODUCT_RELATED_PRODUCT_CATEGORY('Interface component A',
'Interface component A',(#35125));
#35089=PRODUCT_RELATED_PRODUCT_CATEGORY('Motor Stator Face 1',
'Motor Stator Face 1',(#35126));
#35090=PRODUCT_RELATED_PRODUCT_CATEGORY('Motor Plastic Spacer Right',
'Motor Plastic Spacer Right',(#35127));
#35091=PRODUCT_RELATED_PRODUCT_CATEGORY('Motor Plastic Cover 1',
'Motor Plastic Cover 1',(#35128));
#35092=PRODUCT_RELATED_PRODUCT_CATEGORY('Motor Shaft 1','Motor Shaft 1',
(#35129));
#35093=PRODUCT_RELATED_PRODUCT_CATEGORY('Motor Base Cap',
'Motor Base Cap',(#35130));
#35094=PRODUCT_RELATED_PRODUCT_CATEGORY('Interface component D',
'Interface component D',(#35131));
#35095=PRODUCT_RELATED_PRODUCT_CATEGORY('Socket Screw 1',
'Socket Screw 1',(#35132));
#35096=PRODUCT_RELATED_PRODUCT_CATEGORY('Socket Screw 2',
'Socket Screw 2',(#35133));
#35097=PRODUCT_RELATED_PRODUCT_CATEGORY(
'External Shaft Retaining Ring Clip',
'External Shaft Retaining Ring Clip',(#35134));
#35098=PRODUCT_RELATED_PRODUCT_CATEGORY('Motor Stator Face 2',
'Motor Stator Face 2',(#35135));
#35099=PRODUCT_RELATED_PRODUCT_CATEGORY('Motor Top Cap','Motor Top Cap',
(#35136));
#35100=PRODUCT_RELATED_PRODUCT_CATEGORY('Motor Stator Face 3',
'Motor Stator Face 3',(#35137));
#35101=PRODUCT_RELATED_PRODUCT_CATEGORY('Motor Shaft 2','Motor Shaft 2',
(#35138));
#35102=PRODUCT_RELATED_PRODUCT_CATEGORY('Motor Plastic Protector',
'Motor Plastic Protector',(#35139));
#35103=PRODUCT_RELATED_PRODUCT_CATEGORY('Motor PCB','Motor PCB',(#35140));
#35104=PRODUCT_RELATED_PRODUCT_CATEGORY('Socket Screw 3',
'Socket Screw 3',(#35141));
#35105=PRODUCT_RELATED_PRODUCT_CATEGORY('Motor Stator Face 4',
'Motor Stator Face 4',(#35142));
#35106=PRODUCT_RELATED_PRODUCT_CATEGORY('Motor Plastic Spacer Left',
'Motor Plastic Spacer Left',(#35143));
#35107=PRODUCT_RELATED_PRODUCT_CATEGORY('Socket Screw 4',
'Socket Screw 4',(#35144));
#35108=PRODUCT_RELATED_PRODUCT_CATEGORY('Motor Shaft 3','Motor Shaft 3',
(#35145));
#35109=PRODUCT_RELATED_PRODUCT_CATEGORY('Interface component B',
'Interface component B',(#35146));
#35110=PRODUCT_RELATED_PRODUCT_CATEGORY('Motor Stator Face 5',
'Motor Stator Face 5',(#35147));
#35111=PRODUCT_RELATED_PRODUCT_CATEGORY('Socket Screw 5',
'Socket Screw 5',(#35148));
#35112=PRODUCT_RELATED_PRODUCT_CATEGORY('Motor Central Spacer',
'Motor Central Spacer',(#35149));
#35113=PRODUCT_RELATED_PRODUCT_CATEGORY('Motor Stator Face 6',
'Motor Stator Face 6',(#35150));
#35114=PRODUCT_RELATED_PRODUCT_CATEGORY('Socket Screw 6',
'Socket Screw 6',(#35151));
#35115=PRODUCT_RELATED_PRODUCT_CATEGORY('Motor Shaft 4','Motor Shaft 4',
(#35152));
#35116=PRODUCT_RELATED_PRODUCT_CATEGORY('Motor Stator Face 7',
'Motor Stator Face 7',(#35153));
#35117=PRODUCT_RELATED_PRODUCT_CATEGORY('Motor Stator Face 8',
'Motor Stator Face 8',(#35154));
#35118=PRODUCT_RELATED_PRODUCT_CATEGORY('Interface component C',
'Interface component C',(#35155));
#35119=PRODUCT_RELATED_PRODUCT_CATEGORY('Socket Screw 7',
'Socket Screw 7',(#35156));
#35120=PRODUCT_RELATED_PRODUCT_CATEGORY('Pan Head Screw M3x25 1',
'Pan Head Screw M3x25 1',(#35157));
#35121=APPLICATION_PROTOCOL_DEFINITION('international standard',
'ap242_managed_model_based_3d_engineering',2011,#35122);
#35122=APPLICATION_CONTEXT('Managed model based 3d engineering');
#35123=PRODUCT_CONTEXT('part definition',#35122,'mechanical');
#35124=PRODUCT('Stepper Motor Reference Model',
'MAT-073',
'LEGAL AND USAGE DISCLAIMER: this Data/Model is provided \X2\201C\X0\A
S IS\X2\201D\X0\ for informational and representational only. It is a 
geometric approximation and is NOT engineered, certified, or guarantee
d for dimensional accuracy, exact tolerances, or production-level prec
ision. Vendor disclaims all implied warranties including fitness for a
 particular purpose. DO NOT USE FOR DIRECT PHYSICAL MANUFACTURING, AUT
OMATED PRODUCTION, OR SAFETY-CRITICAL SYSTEMS without independent engi
neering verification and resolution of any design discrepancies.',(#35123));
#35125=PRODUCT('Interface component A','Interface component A',
'LEGAL AND USAGE DISCLAIMER: this Data/Model is provided \X2\201C\X0\A
S IS\X2\201D\X0\ for informational and representational only. It is a 
geometric approximation and is NOT engineered, certified, or guarantee
d for dimensional accuracy, exact tolerances, or production-level prec
ision. Vendor disclaims all implied warranties including fitness for a
 particular purpose. DO NOT USE FOR DIRECT PHYSICAL MANUFACTURING, AUT
OMATED PRODUCTION, OR SAFETY-CRITICAL SYSTEMS without independent engi
neering verification and resolution of any design discrepancies.',(#35123));
#35126=PRODUCT('Motor Stator Face 1','Motor Stator Face 1',
'LEGAL AND USAGE DISCLAIMER: this Data/Model is provided \X2\201C\X0\A
S IS\X2\201D\X0\ for informational and representational only. It is a 
geometric approximation and is NOT engineered, certified, or guarantee
d for dimensional accuracy, exact tolerances, or production-level prec
ision. Vendor disclaims all implied warranties including fitness for a
 particular purpose. DO NOT USE FOR DIRECT PHYSICAL MANUFACTURING, AUT
OMATED PRODUCTION, OR SAFETY-CRITICAL SYSTEMS without independent engi
neering verification and resolution of any design discrepancies.',(#35123));
#35127=PRODUCT('Motor Plastic Spacer Right',
'Motor Plastic Spacer Right',
'LEGAL AND USAGE DISCLAIMER: this Data/Model is provided \X2\201C\X0\A
S IS\X2\201D\X0\ for informational and representational only. It is a 
geometric approximation and is NOT engineered, certified, or guarantee
d for dimensional accuracy, exact tolerances, or production-level prec
ision. Vendor disclaims all implied warranties including fitness for a
 particular purpose. DO NOT USE FOR DIRECT PHYSICAL MANUFACTURING, AUT
OMATED PRODUCTION, OR SAFETY-CRITICAL SYSTEMS without independent engi
neering verification and resolution of any design discrepancies.',(#35123));
#35128=PRODUCT('Motor Plastic Cover 1','Motor Plastic Cover 1',
'LEGAL AND USAGE DISCLAIMER: this Data/Model is provided \X2\201C\X0\A
S IS\X2\201D\X0\ for informational and representational only. It is a 
geometric approximation and is NOT engineered, certified, or guarantee
d for dimensional accuracy, exact tolerances, or production-level prec
ision. Vendor disclaims all implied warranties including fitness for a
 particular purpose. DO NOT USE FOR DIRECT PHYSICAL MANUFACTURING, AUT
OMATED PRODUCTION, OR SAFETY-CRITICAL SYSTEMS without independent engi
neering verification and resolution of any design discrepancies.',(#35123));
#35129=PRODUCT('Motor Shaft 1','Motor Shaft 1',
'LEGAL AND USAGE DISCLAIMER: this Data/Model is provided \X2\201C\X0\A
S IS\X2\201D\X0\ for informational and representational only. It is a 
geometric approximation and is NOT engineered, certified, or guarantee
d for dimensional accuracy, exact tolerances, or production-level prec
ision. Vendor disclaims all implied warranties including fitness for a
 particular purpose. DO NOT USE FOR DIRECT PHYSICAL MANUFACTURING, AUT
OMATED PRODUCTION, OR SAFETY-CRITICAL SYSTEMS without independent engi
neering verification and resolution of any design discrepancies.',(#35123));
#35130=PRODUCT('Motor Base Cap','Motor Base Cap',
'LEGAL AND USAGE DISCLAIMER: this Data/Model is provided \X2\201C\X0\A
S IS\X2\201D\X0\ for informational and representational only. It is a 
geometric approximation and is NOT engineered, certified, or guarantee
d for dimensional accuracy, exact tolerances, or production-level prec
ision. Vendor disclaims all implied warranties including fitness for a
 particular purpose. DO NOT USE FOR DIRECT PHYSICAL MANUFACTURING, AUT
OMATED PRODUCTION, OR SAFETY-CRITICAL SYSTEMS without independent engi
neering verification and resolution of any design discrepancies.',(#35123));
#35131=PRODUCT('Interface component D','Interface component D',
'LEGAL AND USAGE DISCLAIMER: this Data/Model is provided \X2\201C\X0\A
S IS\X2\201D\X0\ for informational and representational only. It is a 
geometric approximation and is NOT engineered, certified, or guarantee
d for dimensional accuracy, exact tolerances, or production-level prec
ision. Vendor disclaims all implied warranties including fitness for a
 particular purpose. DO NOT USE FOR DIRECT PHYSICAL MANUFACTURING, AUT
OMATED PRODUCTION, OR SAFETY-CRITICAL SYSTEMS without independent engi
neering verification and resolution of any design discrepancies.',(#35123));
#35132=PRODUCT('Socket Screw 1','Socket Screw 1',
'LEGAL AND USAGE DISCLAIMER: this Data/Model is provided \X2\201C\X0\A
S IS\X2\201D\X0\ for informational and representational only. It is a 
geometric approximation and is NOT engineered, certified, or guarantee
d for dimensional accuracy, exact tolerances, or production-level prec
ision. Vendor disclaims all implied warranties including fitness for a
 particular purpose. DO NOT USE FOR DIRECT PHYSICAL MANUFACTURING, AUT
OMATED PRODUCTION, OR SAFETY-CRITICAL SYSTEMS without independent engi
neering verification and resolution of any design discrepancies.',(#35123));
#35133=PRODUCT('Socket Screw 2','Socket Screw 2',
'LEGAL AND USAGE DISCLAIMER: this Data/Model is provided \X2\201C\X0\A
S IS\X2\201D\X0\ for informational and representational only. It is a 
geometric approximation and is NOT engineered, certified, or guarantee
d for dimensional accuracy, exact tolerances, or production-level prec
ision. Vendor disclaims all implied warranties including fitness for a
 particular purpose. DO NOT USE FOR DIRECT PHYSICAL MANUFACTURING, AUT
OMATED PRODUCTION, OR SAFETY-CRITICAL SYSTEMS without independent engi
neering verification and resolution of any design discrepancies.',(#35123));
#35134=PRODUCT('External Shaft Retaining Ring Clip',
'External Shaft Retaining Ring Clip',
'LEGAL AND USAGE DISCLAIMER: this Data/Model is provided \X2\201C\X0\A
S IS\X2\201D\X0\ for informational and representational only. It is a 
geometric approximation and is NOT engineered, certified, or guarantee
d for dimensional accuracy, exact tolerances, or production-level prec
ision. Vendor disclaims all implied warranties including fitness for a
 particular purpose. DO NOT USE FOR DIRECT PHYSICAL MANUFACTURING, AUT
OMATED PRODUCTION, OR SAFETY-CRITICAL SYSTEMS without independent engi
neering verification and resolution of any design discrepancies.',(#35123));
#35135=PRODUCT('Motor Stator Face 2','Motor Stator Face 2',
'LEGAL AND USAGE DISCLAIMER: this Data/Model is provided \X2\201C\X0\A
S IS\X2\201D\X0\ for informational and representational only. It is a 
geometric approximation and is NOT engineered, certified, or guarantee
d for dimensional accuracy, exact tolerances, or production-level prec
ision. Vendor disclaims all implied warranties including fitness for a
 particular purpose. DO NOT USE FOR DIRECT PHYSICAL MANUFACTURING, AUT
OMATED PRODUCTION, OR SAFETY-CRITICAL SYSTEMS without independent engi
neering verification and resolution of any design discrepancies.',(#35123));
#35136=PRODUCT('Motor Top Cap','Motor Top Cap',
'LEGAL AND USAGE DISCLAIMER: this Data/Model is provided \X2\201C\X0\A
S IS\X2\201D\X0\ for informational and representational only. It is a 
geometric approximation and is NOT engineered, certified, or guarantee
d for dimensional accuracy, exact tolerances, or production-level prec
ision. Vendor disclaims all implied warranties including fitness for a
 particular purpose. DO NOT USE FOR DIRECT PHYSICAL MANUFACTURING, AUT
OMATED PRODUCTION, OR SAFETY-CRITICAL SYSTEMS without independent engi
neering verification and resolution of any design discrepancies.',(#35123));
#35137=PRODUCT('Motor Stator Face 3','Motor Stator Face 3',
'LEGAL AND USAGE DISCLAIMER: this Data/Model is provided \X2\201C\X0\A
S IS\X2\201D\X0\ for informational and representational only. It is a 
geometric approximation and is NOT engineered, certified, or guarantee
d for dimensional accuracy, exact tolerances, or production-level prec
ision. Vendor disclaims all implied warranties including fitness for a
 particular purpose. DO NOT USE FOR DIRECT PHYSICAL MANUFACTURING, AUT
OMATED PRODUCTION, OR SAFETY-CRITICAL SYSTEMS without independent engi
neering verification and resolution of any design discrepancies.',(#35123));
#35138=PRODUCT('Motor Shaft 2','Motor Shaft 2',
'LEGAL AND USAGE DISCLAIMER: this Data/Model is provided \X2\201C\X0\A
S IS\X2\201D\X0\ for informational and representational only. It is a 
geometric approximation and is NOT engineered, certified, or guarantee
d for dimensional accuracy, exact tolerances, or production-level prec
ision. Vendor disclaims all implied warranties including fitness for a
 particular purpose. DO NOT USE FOR DIRECT PHYSICAL MANUFACTURING, AUT
OMATED PRODUCTION, OR SAFETY-CRITICAL SYSTEMS without independent engi
neering verification and resolution of any design discrepancies.',(#35123));
#35139=PRODUCT('Motor Plastic Protector','Motor Plastic Protector',
'LEGAL AND USAGE DISCLAIMER: this Data/Model is provided \X2\201C\X0\A
S IS\X2\201D\X0\ for informational and representational only. It is a 
geometric approximation and is NOT engineered, certified, or guarantee
d for dimensional accuracy, exact tolerances, or production-level prec
ision. Vendor disclaims all implied warranties including fitness for a
 particular purpose. DO NOT USE FOR DIRECT PHYSICAL MANUFACTURING, AUT
OMATED PRODUCTION, OR SAFETY-CRITICAL SYSTEMS without independent engi
neering verification and resolution of any design discrepancies.',(#35123));
#35140=PRODUCT('Motor PCB','Motor PCB',
'LEGAL AND USAGE DISCLAIMER: this Data/Model is provided \X2\201C\X0\A
S IS\X2\201D\X0\ for informational and representational only. It is a 
geometric approximation and is NOT engineered, certified, or guarantee
d for dimensional accuracy, exact tolerances, or production-level prec
ision. Vendor disclaims all implied warranties including fitness for a
 particular purpose. DO NOT USE FOR DIRECT PHYSICAL MANUFACTURING, AUT
OMATED PRODUCTION, OR SAFETY-CRITICAL SYSTEMS without independent engi
neering verification and resolution of any design discrepancies.',(#35123));
#35141=PRODUCT('Socket Screw 3','Socket Screw 3',
'LEGAL AND USAGE DISCLAIMER: this Data/Model is provided \X2\201C\X0\A
S IS\X2\201D\X0\ for informational and representational only. It is a 
geometric approximation and is NOT engineered, certified, or guarantee
d for dimensional accuracy, exact tolerances, or production-level prec
ision. Vendor disclaims all implied warranties including fitness for a
 particular purpose. DO NOT USE FOR DIRECT PHYSICAL MANUFACTURING, AUT
OMATED PRODUCTION, OR SAFETY-CRITICAL SYSTEMS without independent engi
neering verification and resolution of any design discrepancies.',(#35123));
#35142=PRODUCT('Motor Stator Face 4','Motor Stator Face 4',
'LEGAL AND USAGE DISCLAIMER: this Data/Model is provided \X2\201C\X0\A
S IS\X2\201D\X0\ for informational and representational only. It is a 
geometric approximation and is NOT engineered, certified, or guarantee
d for dimensional accuracy, exact tolerances, or production-level prec
ision. Vendor disclaims all implied warranties including fitness for a
 particular purpose. DO NOT USE FOR DIRECT PHYSICAL MANUFACTURING, AUT
OMATED PRODUCTION, OR SAFETY-CRITICAL SYSTEMS without independent engi
neering verification and resolution of any design discrepancies.',(#35123));
#35143=PRODUCT('Motor Plastic Spacer Left','Motor Plastic Spacer Left',

'LEGAL AND USAGE DISCLAIMER: this Data/Model is provided \X2\201C\X0\A
S IS\X2\201D\X0\ for informational and representational only. It is a 
geometric approximation and is NOT engineered, certified, or guarantee
d for dimensional accuracy, exact tolerances, or production-level prec
ision. Vendor disclaims all implied warranties including fitness for a
 particular purpose. DO NOT USE FOR DIRECT PHYSICAL MANUFACTURING, AUT
OMATED PRODUCTION, OR SAFETY-CRITICAL SYSTEMS without independent engi
neering verification and resolution of any design discrepancies.',(#35123));
#35144=PRODUCT('Socket Screw 4','Socket Screw 4',
'LEGAL AND USAGE DISCLAIMER: this Data/Model is provided \X2\201C\X0\A
S IS\X2\201D\X0\ for informational and representational only. It is a 
geometric approximation and is NOT engineered, certified, or guarantee
d for dimensional accuracy, exact tolerances, or production-level prec
ision. Vendor disclaims all implied warranties including fitness for a
 particular purpose. DO NOT USE FOR DIRECT PHYSICAL MANUFACTURING, AUT
OMATED PRODUCTION, OR SAFETY-CRITICAL SYSTEMS without independent engi
neering verification and resolution of any design discrepancies.',(#35123));
#35145=PRODUCT('Motor Shaft 3','Motor Shaft 3',
'LEGAL AND USAGE DISCLAIMER: this Data/Model is provided \X2\201C\X0\A
S IS\X2\201D\X0\ for informational and representational only. It is a 
geometric approximation and is NOT engineered, certified, or guarantee
d for dimensional accuracy, exact tolerances, or production-level prec
ision. Vendor disclaims all implied warranties including fitness for a
 particular purpose. DO NOT USE FOR DIRECT PHYSICAL MANUFACTURING, AUT
OMATED PRODUCTION, OR SAFETY-CRITICAL SYSTEMS without independent engi
neering verification and resolution of any design discrepancies.',(#35123));
#35146=PRODUCT('Interface component B','Interface component B',
'LEGAL AND USAGE DISCLAIMER: this Data/Model is provided \X2\201C\X0\A
S IS\X2\201D\X0\ for informational and representational only. It is a 
geometric approximation and is NOT engineered, certified, or guarantee
d for dimensional accuracy, exact tolerances, or production-level prec
ision. Vendor disclaims all implied warranties including fitness for a
 particular purpose. DO NOT USE FOR DIRECT PHYSICAL MANUFACTURING, AUT
OMATED PRODUCTION, OR SAFETY-CRITICAL SYSTEMS without independent engi
neering verification and resolution of any design discrepancies.',(#35123));
#35147=PRODUCT('Motor Stator Face 5','Motor Stator Face 5',
'LEGAL AND USAGE DISCLAIMER: this Data/Model is provided \X2\201C\X0\A
S IS\X2\201D\X0\ for informational and representational only. It is a 
geometric approximation and is NOT engineered, certified, or guarantee
d for dimensional accuracy, exact tolerances, or production-level prec
ision. Vendor disclaims all implied warranties including fitness for a
 particular purpose. DO NOT USE FOR DIRECT PHYSICAL MANUFACTURING, AUT
OMATED PRODUCTION, OR SAFETY-CRITICAL SYSTEMS without independent engi
neering verification and resolution of any design discrepancies.',(#35123));
#35148=PRODUCT('Socket Screw 5','Socket Screw 5',
'LEGAL AND USAGE DISCLAIMER: this Data/Model is provided \X2\201C\X0\A
S IS\X2\201D\X0\ for informational and representational only. It is a 
geometric approximation and is NOT engineered, certified, or guarantee
d for dimensional accuracy, exact tolerances, or production-level prec
ision. Vendor disclaims all implied warranties including fitness for a
 particular purpose. DO NOT USE FOR DIRECT PHYSICAL MANUFACTURING, AUT
OMATED PRODUCTION, OR SAFETY-CRITICAL SYSTEMS without independent engi
neering verification and resolution of any design discrepancies.',(#35123));
#35149=PRODUCT('Motor Central Spacer','Motor Central Spacer',
'LEGAL AND USAGE DISCLAIMER: this Data/Model is provided \X2\201C\X0\A
S IS\X2\201D\X0\ for informational and representational only. It is a 
geometric approximation and is NOT engineered, certified, or guarantee
d for dimensional accuracy, exact tolerances, or production-level prec
ision. Vendor disclaims all implied warranties including fitness for a
 particular purpose. DO NOT USE FOR DIRECT PHYSICAL MANUFACTURING, AUT
OMATED PRODUCTION, OR SAFETY-CRITICAL SYSTEMS without independent engi
neering verification and resolution of any design discrepancies.',(#35123));
#35150=PRODUCT('Motor Stator Face 6','Motor Stator Face 6',
'LEGAL AND USAGE DISCLAIMER: this Data/Model is provided \X2\201C\X0\A
S IS\X2\201D\X0\ for informational and representational only. It is a 
geometric approximation and is NOT engineered, certified, or guarantee
d for dimensional accuracy, exact tolerances, or production-level prec
ision. Vendor disclaims all implied warranties including fitness for a
 particular purpose. DO NOT USE FOR DIRECT PHYSICAL MANUFACTURING, AUT
OMATED PRODUCTION, OR SAFETY-CRITICAL SYSTEMS without independent engi
neering verification and resolution of any design discrepancies.',(#35123));
#35151=PRODUCT('Socket Screw 6','Socket Screw 6',
'LEGAL AND USAGE DISCLAIMER: this Data/Model is provided \X2\201C\X0\A
S IS\X2\201D\X0\ for informational and representational only. It is a 
geometric approximation and is NOT engineered, certified, or guarantee
d for dimensional accuracy, exact tolerances, or production-level prec
ision. Vendor disclaims all implied warranties including fitness for a
 particular purpose. DO NOT USE FOR DIRECT PHYSICAL MANUFACTURING, AUT
OMATED PRODUCTION, OR SAFETY-CRITICAL SYSTEMS without independent engi
neering verification and resolution of any design discrepancies.',(#35123));
#35152=PRODUCT('Motor Shaft 4','Motor Shaft 4',
'LEGAL AND USAGE DISCLAIMER: this Data/Model is provided \X2\201C\X0\A
S IS\X2\201D\X0\ for informational and representational only. It is a 
geometric approximation and is NOT engineered, certified, or guarantee
d for dimensional accuracy, exact tolerances, or production-level prec
ision. Vendor disclaims all implied warranties including fitness for a
 particular purpose. DO NOT USE FOR DIRECT PHYSICAL MANUFACTURING, AUT
OMATED PRODUCTION, OR SAFETY-CRITICAL SYSTEMS without independent engi
neering verification and resolution of any design discrepancies.',(#35123));
#35153=PRODUCT('Motor Stator Face 7','Motor Stator Face 7',
'LEGAL AND USAGE DISCLAIMER: this Data/Model is provided \X2\201C\X0\A
S IS\X2\201D\X0\ for informational and representational only. It is a 
geometric approximation and is NOT engineered, certified, or guarantee
d for dimensional accuracy, exact tolerances, or production-level prec
ision. Vendor disclaims all implied warranties including fitness for a
 particular purpose. DO NOT USE FOR DIRECT PHYSICAL MANUFACTURING, AUT
OMATED PRODUCTION, OR SAFETY-CRITICAL SYSTEMS without independent engi
neering verification and resolution of any design discrepancies.',(#35123));
#35154=PRODUCT('Motor Stator Face 8','Motor Stator Face 8',
'LEGAL AND USAGE DISCLAIMER: this Data/Model is provided \X2\201C\X0\A
S IS\X2\201D\X0\ for informational and representational only. It is a 
geometric approximation and is NOT engineered, certified, or guarantee
d for dimensional accuracy, exact tolerances, or production-level prec
ision. Vendor disclaims all implied warranties including fitness for a
 particular purpose. DO NOT USE FOR DIRECT PHYSICAL MANUFACTURING, AUT
OMATED PRODUCTION, OR SAFETY-CRITICAL SYSTEMS without independent engi
neering verification and resolution of any design discrepancies.',(#35123));
#35155=PRODUCT('Interface component C','Interface component C',
'LEGAL AND USAGE DISCLAIMER: this Data/Model is provided \X2\201C\X0\A
S IS\X2\201D\X0\ for informational and representational only. It is a 
geometric approximation and is NOT engineered, certified, or guarantee
d for dimensional accuracy, exact tolerances, or production-level prec
ision. Vendor disclaims all implied warranties including fitness for a
 particular purpose. DO NOT USE FOR DIRECT PHYSICAL MANUFACTURING, AUT
OMATED PRODUCTION, OR SAFETY-CRITICAL SYSTEMS without independent engi
neering verification and resolution of any design discrepancies.',(#35123));
#35156=PRODUCT('Socket Screw 7','Socket Screw 7',
'LEGAL AND USAGE DISCLAIMER: this Data/Model is provided \X2\201C\X0\A
S IS\X2\201D\X0\ for informational and representational only. It is a 
geometric approximation and is NOT engineered, certified, or guarantee
d for dimensional accuracy, exact tolerances, or production-level prec
ision. Vendor disclaims all implied warranties including fitness for a
 particular purpose. DO NOT USE FOR DIRECT PHYSICAL MANUFACTURING, AUT
OMATED PRODUCTION, OR SAFETY-CRITICAL SYSTEMS without independent engi
neering verification and resolution of any design discrepancies.',(#35123));
#35157=PRODUCT('Pan Head Screw M3x25 1','Pan Head Screw M3x25 1',
'LEGAL AND USAGE DISCLAIMER: this Data/Model is provided \X2\201C\X0\A
S IS\X2\201D\X0\ for informational and representational only. It is a 
geometric approximation and is NOT engineered, certified, or guarantee
d for dimensional accuracy, exact tolerances, or production-level prec
ision. Vendor disclaims all implied warranties including fitness for a
 particular purpose. DO NOT USE FOR DIRECT PHYSICAL MANUFACTURING, AUT
OMATED PRODUCTION, OR SAFETY-CRITICAL SYSTEMS without independent engi
neering verification and resolution of any design discrepancies.',(#35123));
#35158=PRESENTATION_STYLE_ASSIGNMENT((#35167));
#35159=PRESENTATION_STYLE_ASSIGNMENT((#35168));
#35160=PRESENTATION_STYLE_ASSIGNMENT((#35169));
#35161=PRESENTATION_STYLE_ASSIGNMENT((#35170));
#35162=PRESENTATION_STYLE_ASSIGNMENT((#35171));
#35163=PRESENTATION_STYLE_ASSIGNMENT((#35172));
#35164=PRESENTATION_STYLE_ASSIGNMENT((#35173));
#35165=PRESENTATION_STYLE_ASSIGNMENT((#35174));
#35166=PRESENTATION_STYLE_ASSIGNMENT((#35175));
#35167=SURFACE_STYLE_USAGE(.BOTH.,#35176);
#35168=SURFACE_STYLE_USAGE(.BOTH.,#35177);
#35169=SURFACE_STYLE_USAGE(.BOTH.,#35178);
#35170=SURFACE_STYLE_USAGE(.BOTH.,#35179);
#35171=SURFACE_STYLE_USAGE(.BOTH.,#35180);
#35172=SURFACE_STYLE_USAGE(.BOTH.,#35181);
#35173=SURFACE_STYLE_USAGE(.BOTH.,#35182);
#35174=SURFACE_STYLE_USAGE(.BOTH.,#35183);
#35175=SURFACE_STYLE_USAGE(.BOTH.,#35184);
#35176=SURFACE_SIDE_STYLE('',(#35185));
#35177=SURFACE_SIDE_STYLE('',(#35186));
#35178=SURFACE_SIDE_STYLE('',(#35187));
#35179=SURFACE_SIDE_STYLE('',(#35188));
#35180=SURFACE_SIDE_STYLE('',(#35189));
#35181=SURFACE_SIDE_STYLE('',(#35190));
#35182=SURFACE_SIDE_STYLE('',(#35191));
#35183=SURFACE_SIDE_STYLE('',(#35192));
#35184=SURFACE_SIDE_STYLE('',(#35193));
#35185=SURFACE_STYLE_FILL_AREA(#35194);
#35186=SURFACE_STYLE_FILL_AREA(#35195);
#35187=SURFACE_STYLE_FILL_AREA(#35196);
#35188=SURFACE_STYLE_FILL_AREA(#35197);
#35189=SURFACE_STYLE_FILL_AREA(#35198);
#35190=SURFACE_STYLE_FILL_AREA(#35199);
#35191=SURFACE_STYLE_FILL_AREA(#35200);
#35192=SURFACE_STYLE_FILL_AREA(#35201);
#35193=SURFACE_STYLE_FILL_AREA(#35202);
#35194=FILL_AREA_STYLE('Steel - Satin',(#35203));
#35195=FILL_AREA_STYLE('Paint - Enamel Glossy (White)',(#35204));
#35196=FILL_AREA_STYLE('Plastic - Glossy (Black)',(#35205));
#35197=FILL_AREA_STYLE('Aluminum - Anodized Glossy (Blue)',(#35206));
#35198=FILL_AREA_STYLE('Aluminum - Anodized Glossy (Grey)',(#35207));
#35199=FILL_AREA_STYLE('Plastic - Matte (Black)',(#35208));
#35200=FILL_AREA_STYLE('Plastic - Matte (White)',(#35209));
#35201=FILL_AREA_STYLE('Paint - Metallic (Blue)',(#35210));
#35202=FILL_AREA_STYLE('Paint - Enamel Glossy (Grey)',(#35211));
#35203=FILL_AREA_STYLE_COLOUR('Steel - Satin',#35212);
#35204=FILL_AREA_STYLE_COLOUR('Paint - Enamel Glossy (White)',#35213);
#35205=FILL_AREA_STYLE_COLOUR('Plastic - Glossy (Black)',#35214);
#35206=FILL_AREA_STYLE_COLOUR('Aluminum - Anodized Glossy (Blue)',#35215);
#35207=FILL_AREA_STYLE_COLOUR('Aluminum - Anodized Glossy (Grey)',#35216);
#35208=FILL_AREA_STYLE_COLOUR('Plastic - Matte (Black)',#35217);
#35209=FILL_AREA_STYLE_COLOUR('Plastic - Matte (White)',#35218);
#35210=FILL_AREA_STYLE_COLOUR('Paint - Metallic (Blue)',#35219);
#35211=FILL_AREA_STYLE_COLOUR('Paint - Enamel Glossy (Grey)',#35220);
#35212=COLOUR_RGB('Steel - Satin',0.627450980392157,0.627450980392157,0.627450980392157);
#35213=COLOUR_RGB('Paint - Enamel Glossy (White)',0.964705882352941,0.964705882352941,
0.952941176470588);
#35214=COLOUR_RGB('Plastic - Glossy (Black)',0.0980392156862745,0.0980392156862745,
0.0980392156862745);
#35215=COLOUR_RGB('Aluminum - Anodized Glossy (Blue)',0.349019607843137,
0.584313725490196,0.854901960784314);
#35216=COLOUR_RGB('Aluminum - Anodized Glossy (Grey)',0.537254901960784,
0.537254901960784,0.537254901960784);
#35217=COLOUR_RGB('Plastic - Matte (Black)',0.0980392156862745,0.0980392156862745,
0.0980392156862745);
#35218=COLOUR_RGB('Plastic - Matte (White)',0.964705882352941,0.964705882352941,
0.952941176470588);
#35219=COLOUR_RGB('Paint - Metallic (Blue)',0.188235294117647,0.231372549019608,
0.588235294117647);
#35220=COLOUR_RGB('Paint - Enamel Glossy (Grey)',0.701960784313725,0.701960784313725,
0.701960784313725);
ENDSEC;
END-ISO-10303-21;
